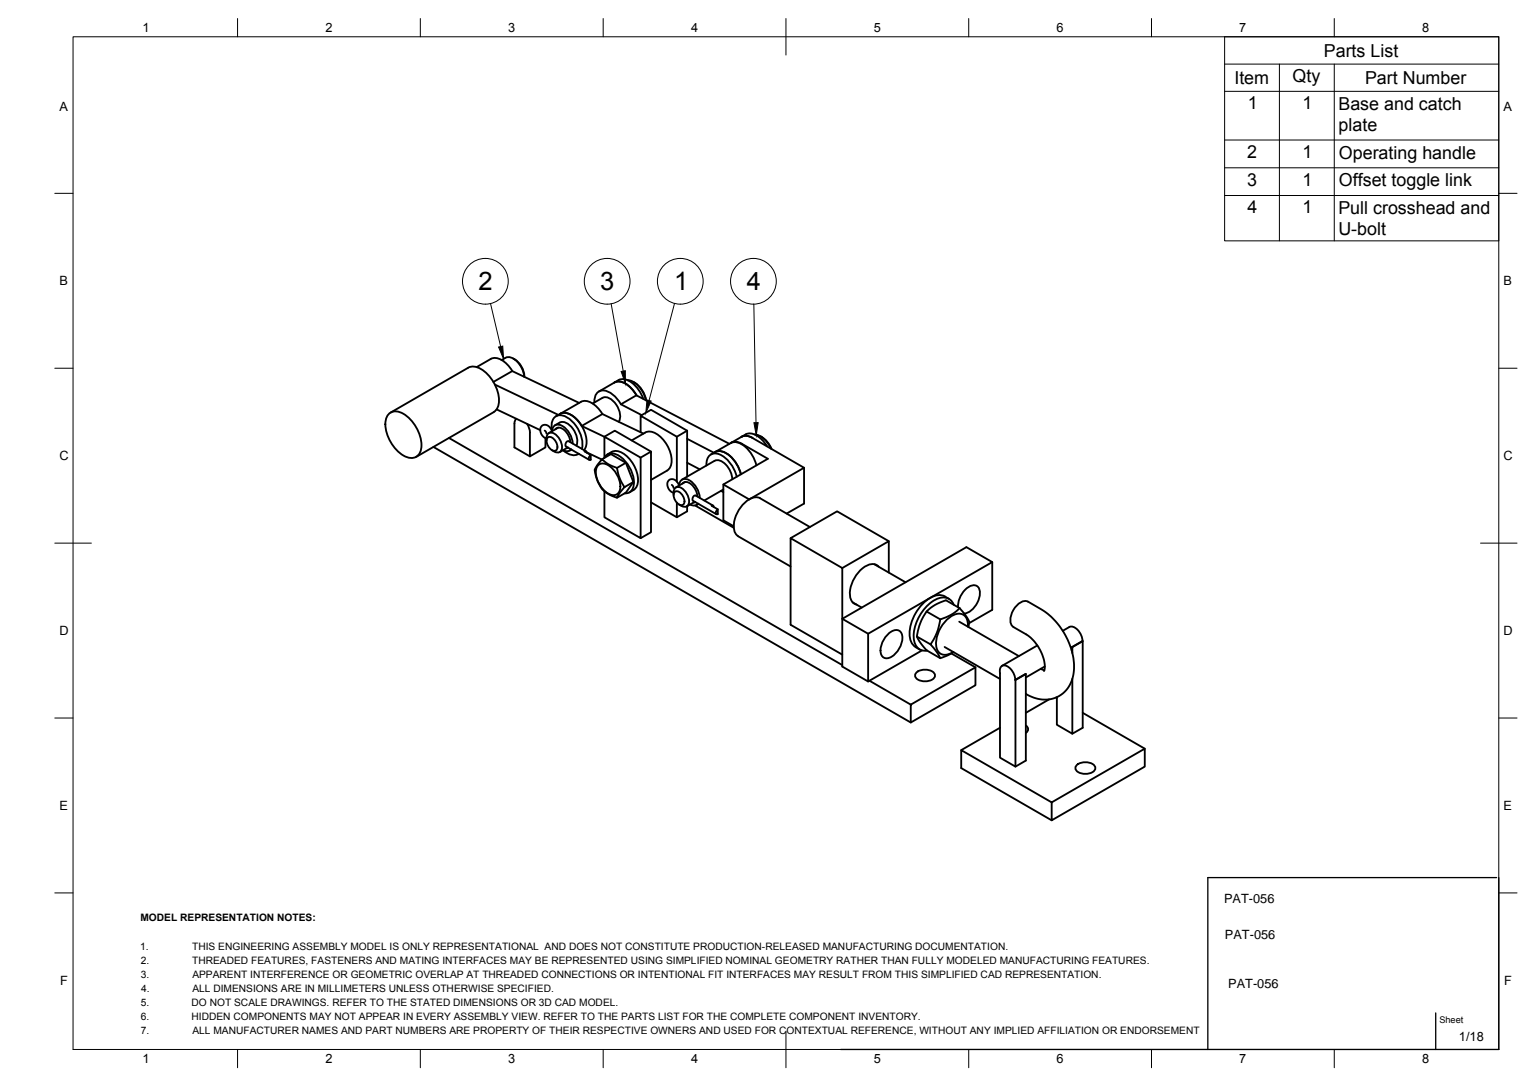
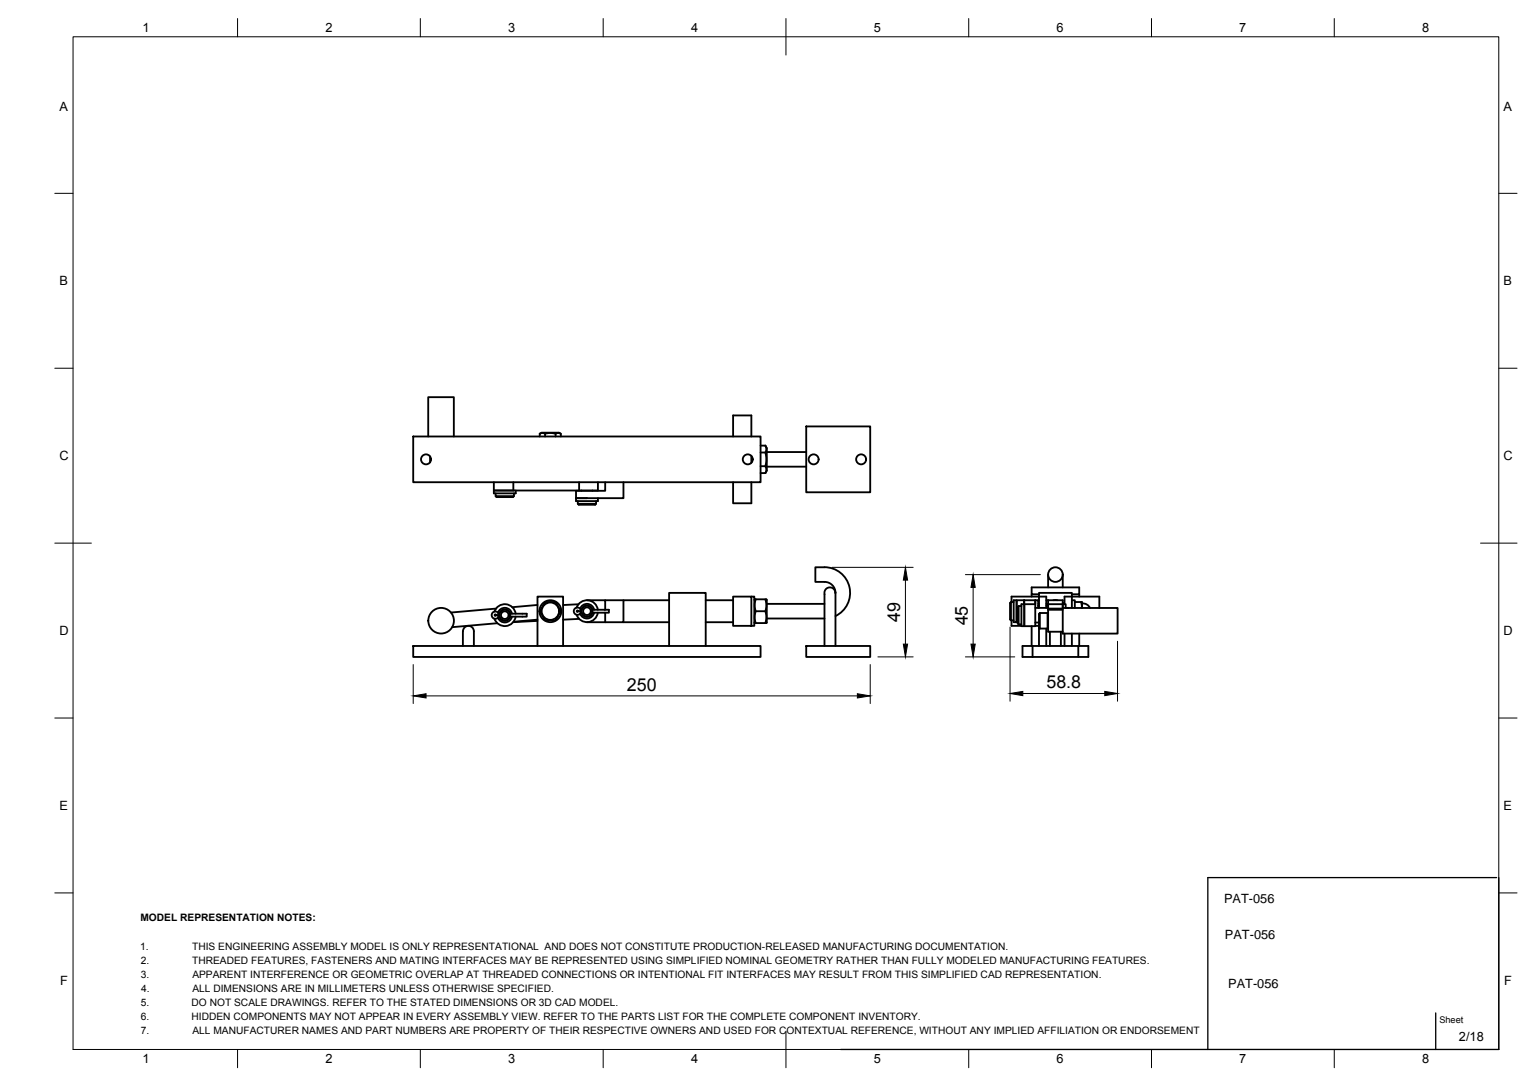
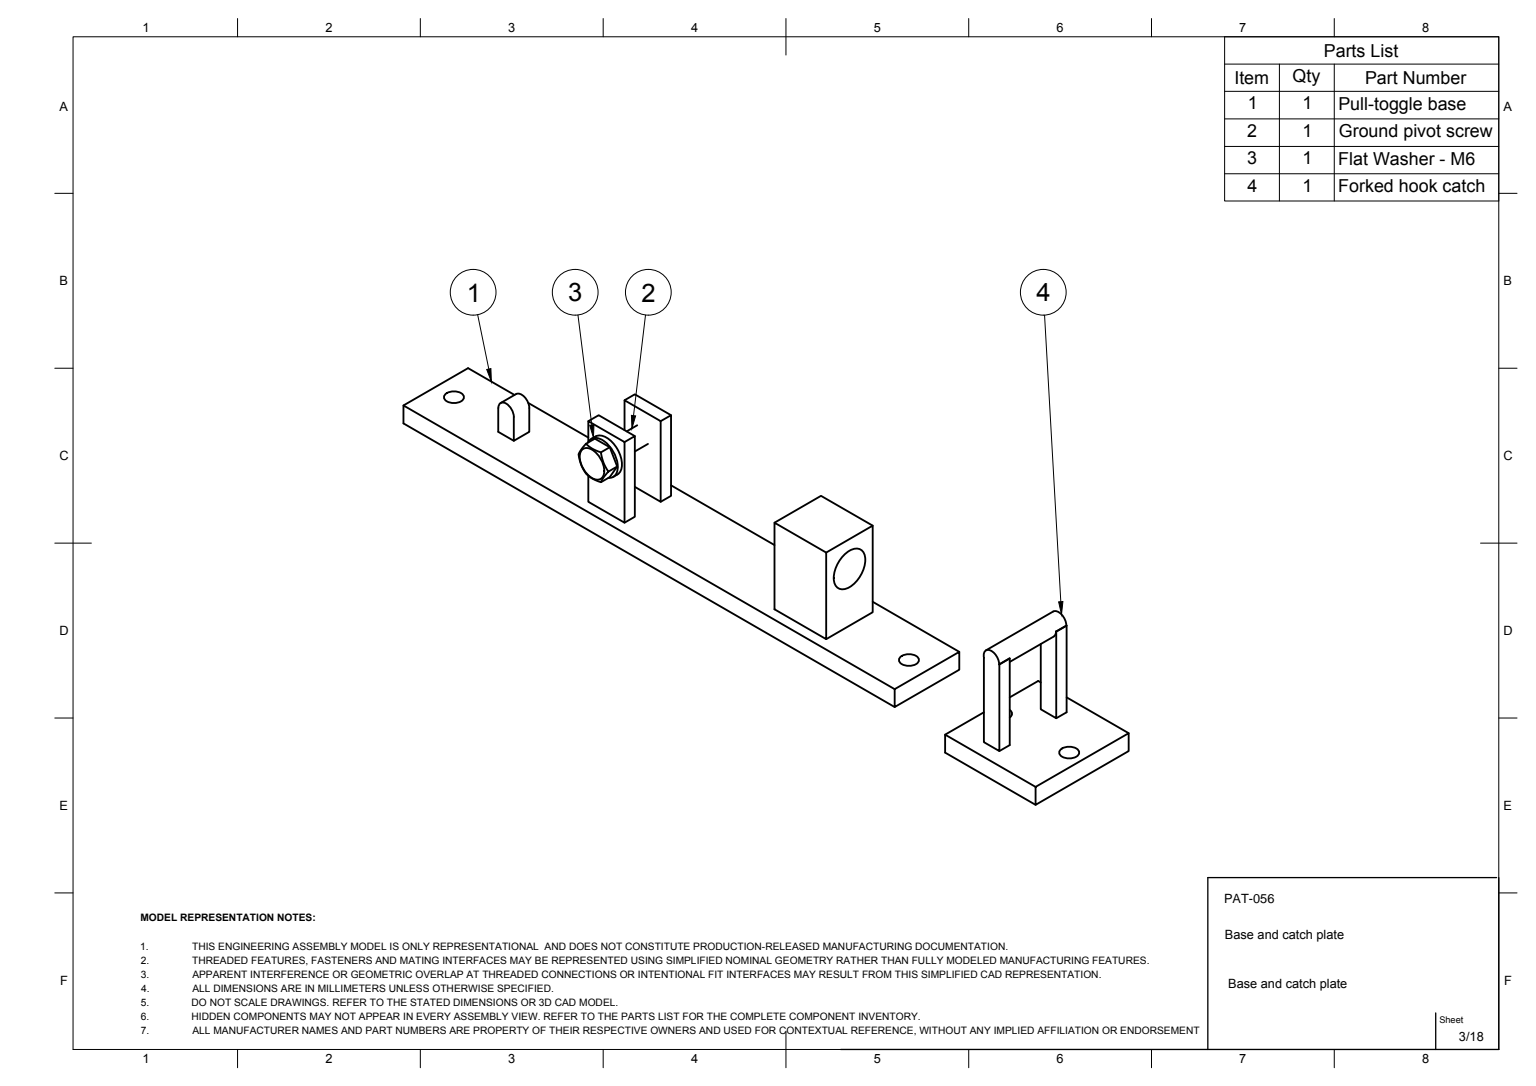
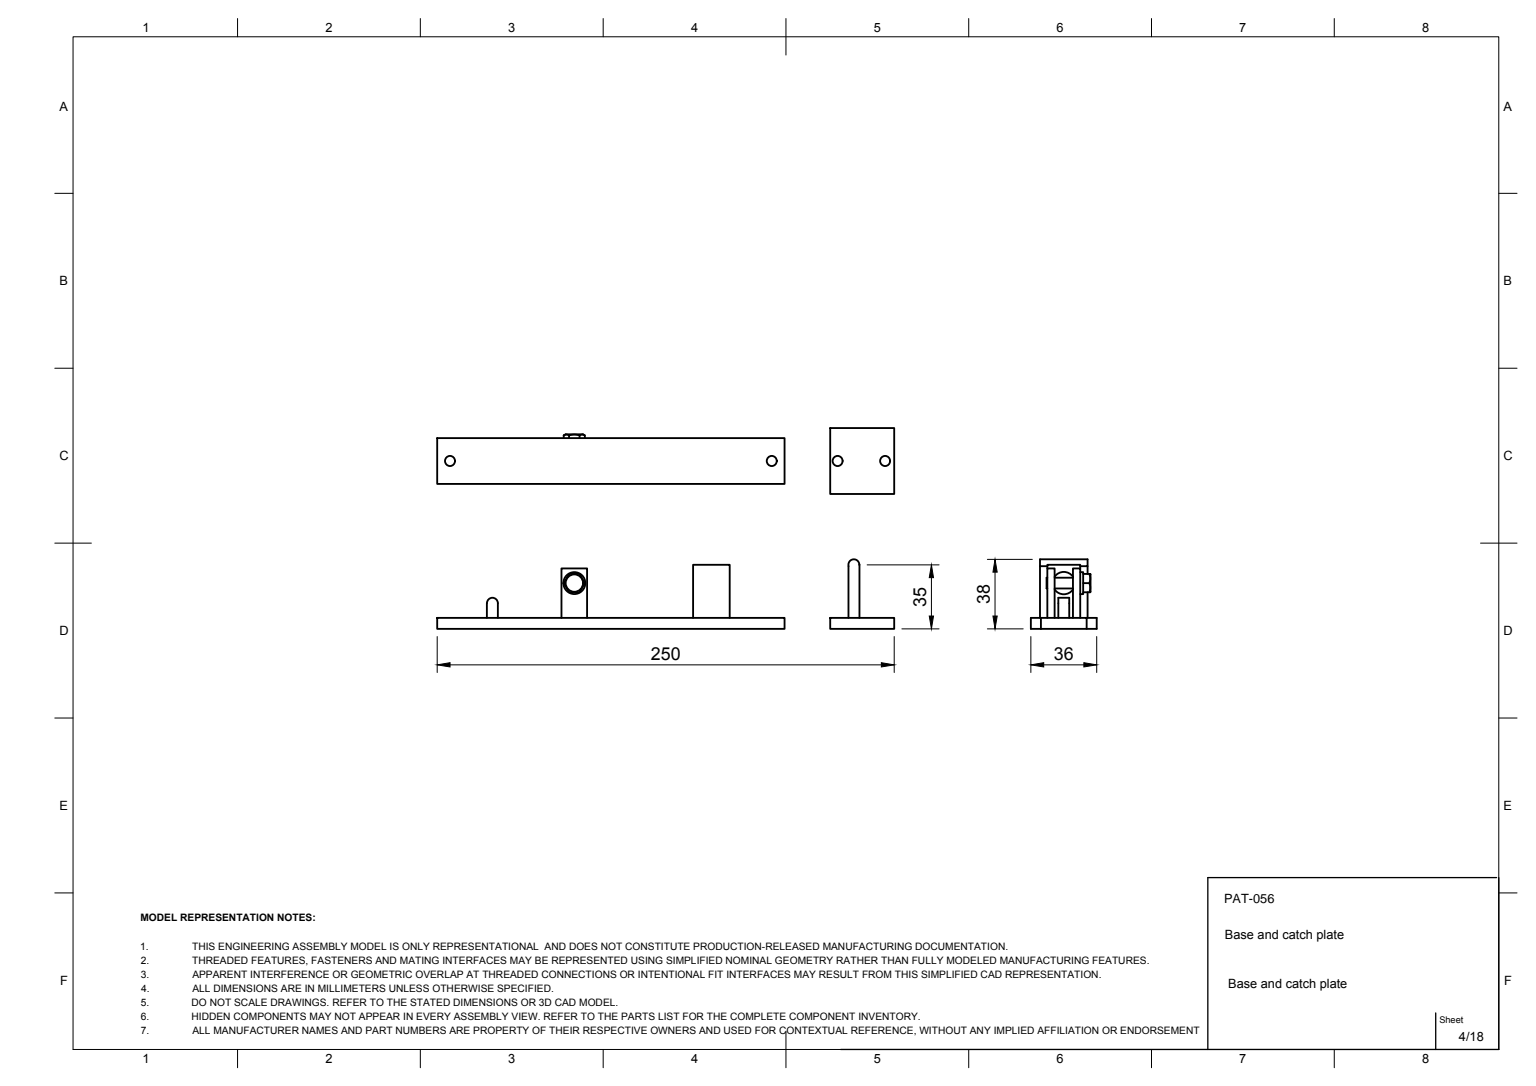
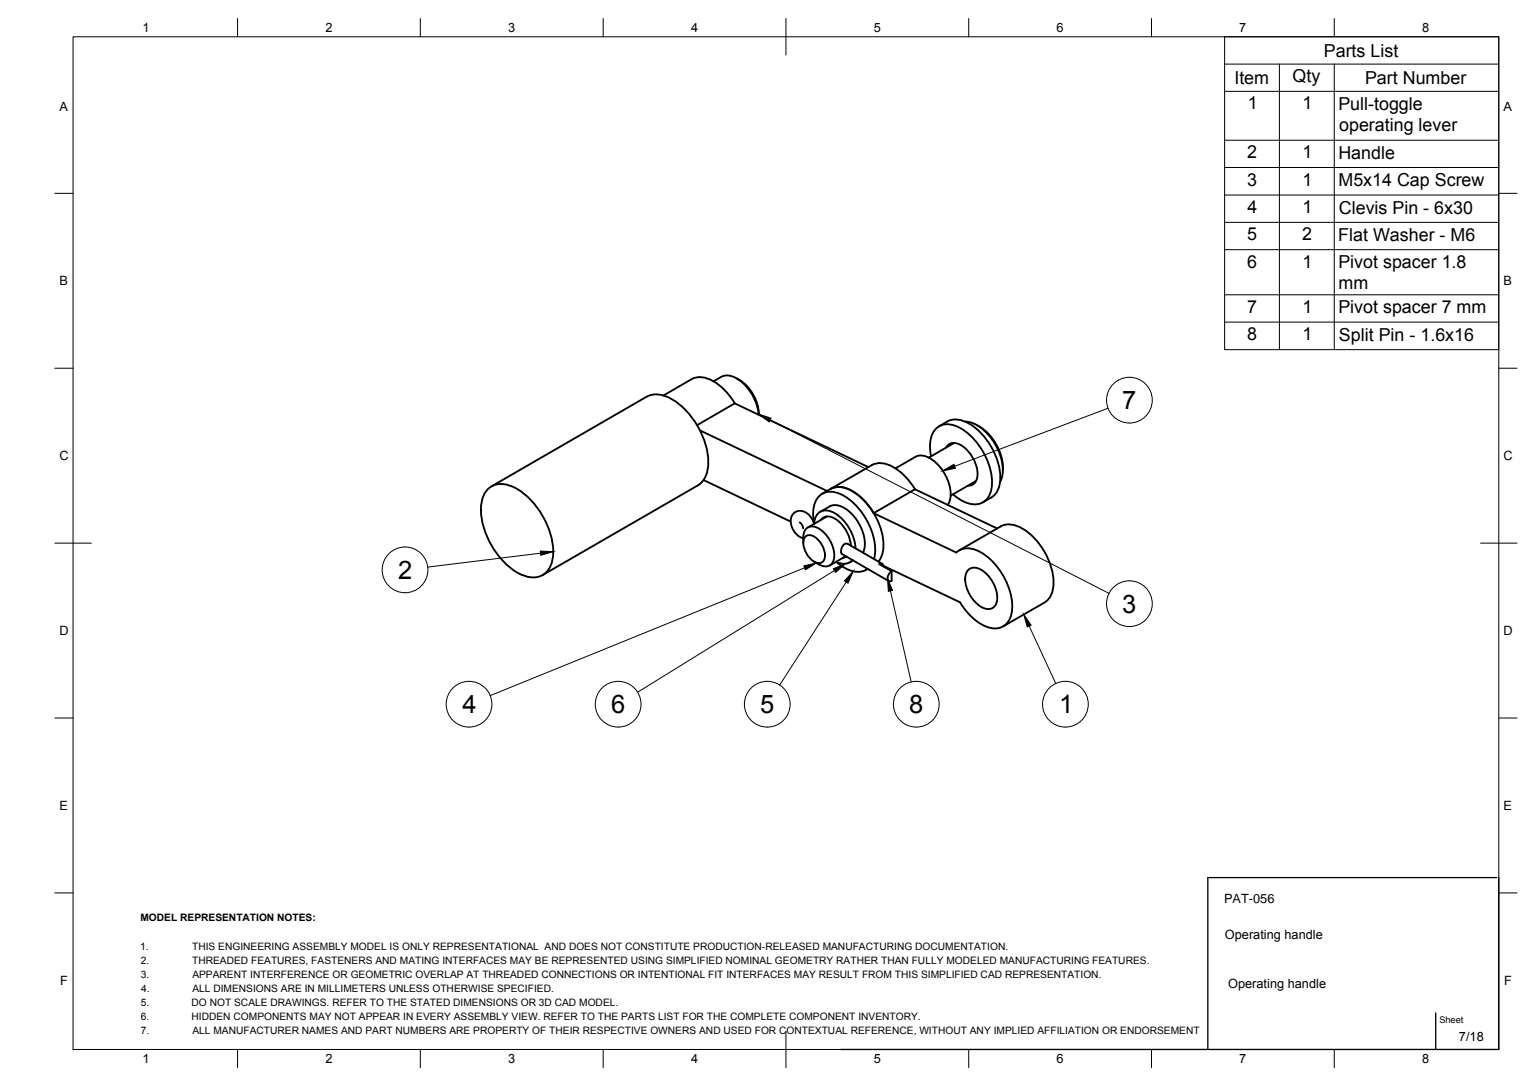
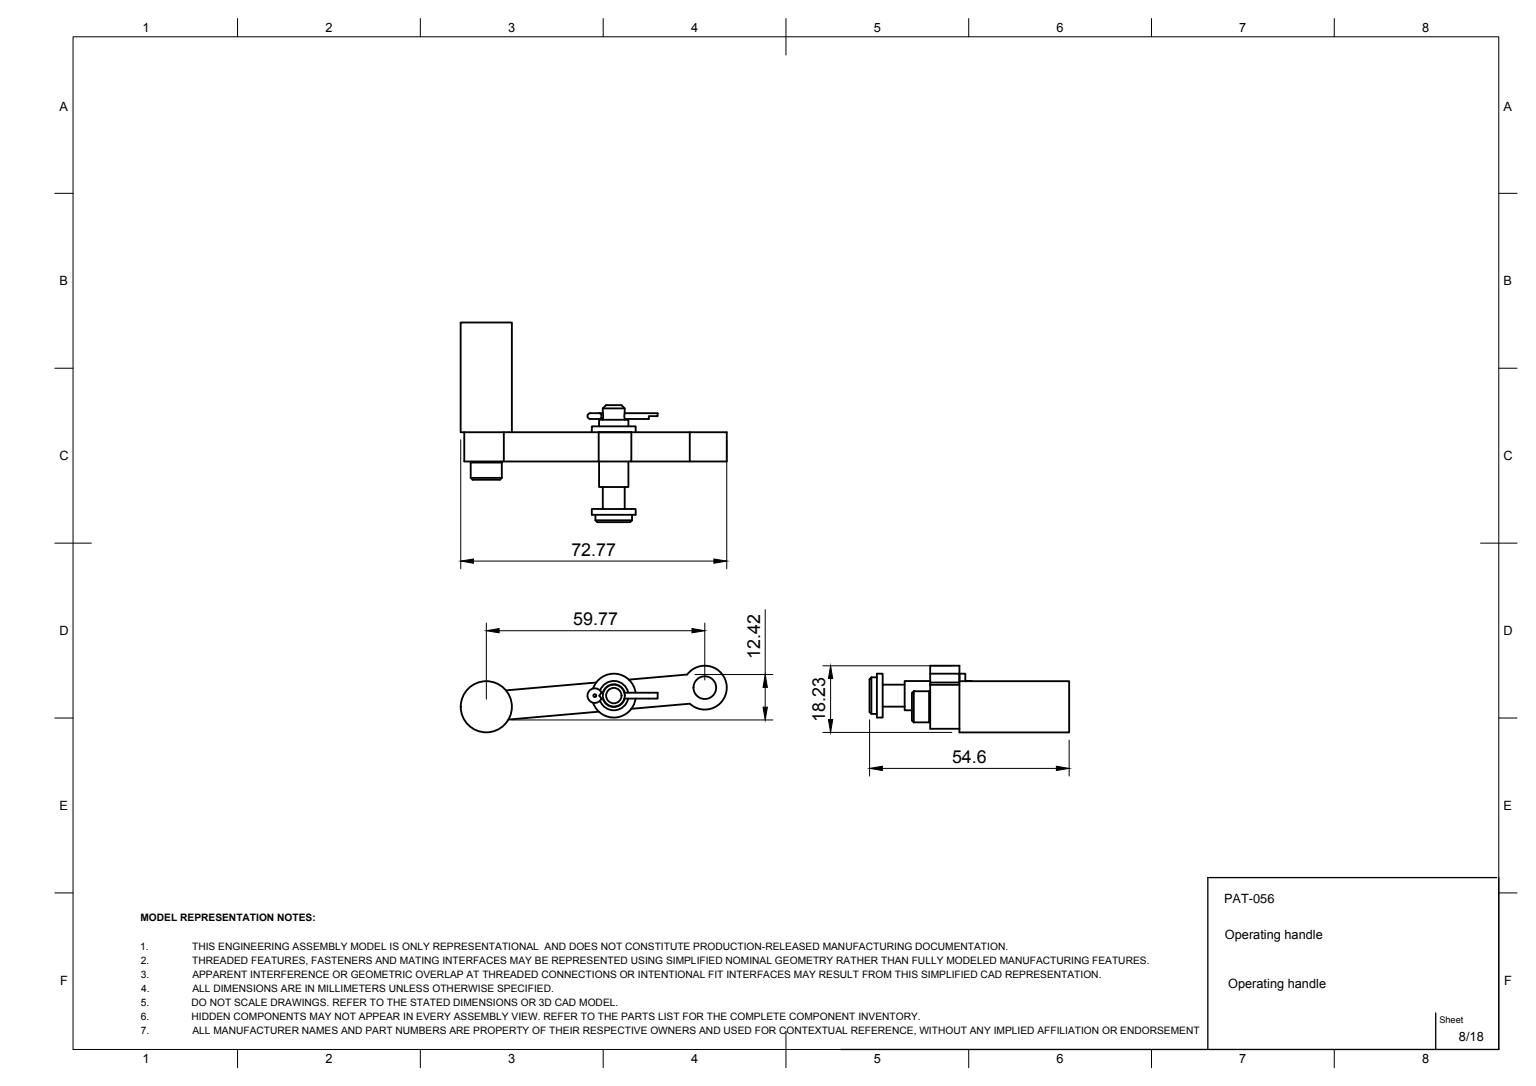
ISO-10303-21;
HEADER;
/* Generated by software containing ST-Developer
 * from STEP Tools, Inc. (www.steptools.com) 
 */

FILE_DESCRIPTION(
/* description */ ('Hook toggle clamp'),
/* implementation_level */ '2;1');

FILE_NAME(
/* name */ 'PAT-056',
/* time_stamp */ '2026-10-27T21:56:56-07:00',
/* author */ (''),
/* organization */ (''),
/* preprocessor_version */ 'ST-DEVELOPER v20.2',
/* originating_system */ 'Autodesk Translation Framework v15.17.0.0',
/* authorisation */ '');

FILE_SCHEMA (('AUTOMOTIVE_DESIGN { 1 0 10303 214 3 1 1 }'));
ENDSEC;

DATA;
#10=MECHANICAL_DESIGN_GEOMETRIC_PRESENTATION_REPRESENTATION('',(#189,#190,
#191,#192,#193,#194,#195,#196,#197,#198,#199,#200,#201,#202,#203,#204,#205),
#5458);
#11=TOROIDAL_SURFACE('',#3441,0.12,0.08);
#12=TOROIDAL_SURFACE('',#3465,1.,0.4);
#13=B_SPLINE_CURVE_WITH_KNOTS('',3,(#5084,#5085,#5086,#5087,#5088,#5089,
#5090,#5091,#5092,#5093),.UNSPECIFIED.,.F.,.F.,(4,2,2,2,4),(0.,0.0302963256060356,
0.0605926512120712,0.090883446720838,0.121174242229605),.UNSPECIFIED.);
#14=B_SPLINE_CURVE_WITH_KNOTS('',3,(#5096,#5097,#5098,#5099,#5100,#5101,
#5102,#5103,#5104,#5105,#5106,#5107,#5108,#5109,#5110,#5111,#5112,#5113,
#5114,#5115,#5116,#5117,#5118,#5119,#5120,#5121,#5122,#5123,#5124,#5125,
#5126,#5127,#5128,#5129),.UNSPECIFIED.,.T.,.F.,(4,2,2,2,2,2,2,2,2,2,2,2,
2,2,2,2,4),(0.,0.0302963256060358,0.0605926512120716,0.0908834467208383,
0.121174242229605,0.151465037738372,0.181755833247138,0.212052158853174,
0.24234848445921,0.272644810065246,0.302941135671282,0.333231931180048,
0.363522726688815,0.393813522197582,0.424104317706349,0.454400643312384,
0.48469696891842),.UNSPECIFIED.);
#15=B_SPLINE_CURVE_WITH_KNOTS('',3,(#5131,#5132,#5133,#5134,#5135,#5136,
#5137,#5138,#5139,#5140),.UNSPECIFIED.,.F.,.F.,(4,2,2,2,4),(0.363522726688815,
0.393813522197581,0.424104317706348,0.454400643312384,0.48469696891842),
 .UNSPECIFIED.);
#16=B_SPLINE_CURVE_WITH_KNOTS('',3,(#5141,#5142,#5143,#5144,#5145,#5146,
#5147,#5148,#5149,#5150,#5151,#5152,#5153,#5154,#5155,#5156,#5157,#5158),
 .UNSPECIFIED.,.F.,.F.,(4,2,2,2,2,2,2,2,4),(0.121174242229605,0.151465037738371,
0.181755833247138,0.212052158853174,0.24234848445921,0.272644810065246,
0.302941135671281,0.333231931180048,0.363522726688815),.UNSPECIFIED.);
#17=B_SPLINE_CURVE_WITH_KNOTS('',3,(#5209,#5210,#5211,#5212,#5213,#5214,
#5215,#5216,#5217,#5218,#5219,#5220,#5221,#5222,#5223,#5224,#5225,#5226,
#5227,#5228,#5229,#5230,#5231,#5232,#5233,#5234),.UNSPECIFIED.,.F.,.F.,
(4,2,2,2,2,2,2,2,2,2,2,2,4),(-0.00054581412719389,0.,0.0281583564005144,
0.0618496465371181,0.0905865724114538,0.120694112793616,0.144966158459363,
0.16923820412511,0.199345744507272,0.228082670381608,0.261773960518212,
0.289932316918681,0.290478131045882),.UNSPECIFIED.);
#18=B_SPLINE_CURVE_WITH_KNOTS('',3,(#5235,#5236,#5237,#5238,#5239,#5240,
#5241,#5242,#5243,#5244,#5245,#5246,#5247,#5248,#5249,#5250,#5251,#5252,
#5253,#5254,#5255,#5256,#5257,#5258,#5259,#5260),.UNSPECIFIED.,.F.,.F.,
(4,2,2,2,2,2,2,2,2,2,2,2,4),(-0.000545814127196571,0.,0.0281583564006391,
0.0618496465374156,0.0905865724118984,0.120694112794215,0.144966158460086,
0.169238204125958,0.199345744508275,0.228082670382758,0.261773960519534,
0.289932316920171,0.29047813104737),.UNSPECIFIED.);
#19=ITEM_DEFINED_TRANSFORMATION($,$,#3349,#3366);
#20=ITEM_DEFINED_TRANSFORMATION($,$,#3178,#3436);
#21=ITEM_DEFINED_TRANSFORMATION($,$,#3222,#3437);
#22=ITEM_DEFINED_TRANSFORMATION($,$,#3427,#3438);
#23=ITEM_DEFINED_TRANSFORMATION($,$,#3237,#3439);
#24=ITEM_DEFINED_TRANSFORMATION($,$,#3268,#3451);
#25=ITEM_DEFINED_TRANSFORMATION($,$,#3296,#3452);
#26=ITEM_DEFINED_TRANSFORMATION($,$,#3305,#3453);
#27=ITEM_DEFINED_TRANSFORMATION($,$,#3314,#3454);
#28=ITEM_DEFINED_TRANSFORMATION($,$,#3324,#3455);
#29=ITEM_DEFINED_TRANSFORMATION($,$,#3412,#3456);
#30=ITEM_DEFINED_TRANSFORMATION($,$,#3427,#3457);
#31=ITEM_DEFINED_TRANSFORMATION($,$,#3427,#3458);
#32=ITEM_DEFINED_TRANSFORMATION($,$,#3440,#3459);
#33=ITEM_DEFINED_TRANSFORMATION($,$,#3368,#3498);
#34=ITEM_DEFINED_TRANSFORMATION($,$,#3403,#3499);
#35=ITEM_DEFINED_TRANSFORMATION($,$,#3412,#3500);
#36=ITEM_DEFINED_TRANSFORMATION($,$,#3427,#3501);
#37=ITEM_DEFINED_TRANSFORMATION($,$,#3427,#3502);
#38=ITEM_DEFINED_TRANSFORMATION($,$,#3440,#3503);
#39=ITEM_DEFINED_TRANSFORMATION($,$,#3460,#3504);
#40=ITEM_DEFINED_TRANSFORMATION($,$,#3473,#3505);
#41=ITEM_DEFINED_TRANSFORMATION($,$,#3482,#3506);
#42=ITEM_DEFINED_TRANSFORMATION($,$,#3177,#3507);
#43=ITEM_DEFINED_TRANSFORMATION($,$,#3267,#3508);
#44=ITEM_DEFINED_TRANSFORMATION($,$,#3348,#3509);
#45=ITEM_DEFINED_TRANSFORMATION($,$,#3367,#3510);
#46=(
REPRESENTATION_RELATIONSHIP($,$,#5546,#5545)
REPRESENTATION_RELATIONSHIP_WITH_TRANSFORMATION(#19)
SHAPE_REPRESENTATION_RELATIONSHIP()
);
#47=(
REPRESENTATION_RELATIONSHIP($,$,#5536,#5535)
REPRESENTATION_RELATIONSHIP_WITH_TRANSFORMATION(#20)
SHAPE_REPRESENTATION_RELATIONSHIP()
);
#48=(
REPRESENTATION_RELATIONSHIP($,$,#5537,#5535)
REPRESENTATION_RELATIONSHIP_WITH_TRANSFORMATION(#21)
SHAPE_REPRESENTATION_RELATIONSHIP()
);
#49=(
REPRESENTATION_RELATIONSHIP($,$,#5551,#5535)
REPRESENTATION_RELATIONSHIP_WITH_TRANSFORMATION(#22)
SHAPE_REPRESENTATION_RELATIONSHIP()
);
#50=(
REPRESENTATION_RELATIONSHIP($,$,#5538,#5535)
REPRESENTATION_RELATIONSHIP_WITH_TRANSFORMATION(#23)
SHAPE_REPRESENTATION_RELATIONSHIP()
);
#51=(
REPRESENTATION_RELATIONSHIP($,$,#5540,#5539)
REPRESENTATION_RELATIONSHIP_WITH_TRANSFORMATION(#24)
SHAPE_REPRESENTATION_RELATIONSHIP()
);
#52=(
REPRESENTATION_RELATIONSHIP($,$,#5541,#5539)
REPRESENTATION_RELATIONSHIP_WITH_TRANSFORMATION(#25)
SHAPE_REPRESENTATION_RELATIONSHIP()
);
#53=(
REPRESENTATION_RELATIONSHIP($,$,#5542,#5539)
REPRESENTATION_RELATIONSHIP_WITH_TRANSFORMATION(#26)
SHAPE_REPRESENTATION_RELATIONSHIP()
);
#54=(
REPRESENTATION_RELATIONSHIP($,$,#5543,#5539)
REPRESENTATION_RELATIONSHIP_WITH_TRANSFORMATION(#27)
SHAPE_REPRESENTATION_RELATIONSHIP()
);
#55=(
REPRESENTATION_RELATIONSHIP($,$,#5544,#5539)
REPRESENTATION_RELATIONSHIP_WITH_TRANSFORMATION(#28)
SHAPE_REPRESENTATION_RELATIONSHIP()
);
#56=(
REPRESENTATION_RELATIONSHIP($,$,#5550,#5539)
REPRESENTATION_RELATIONSHIP_WITH_TRANSFORMATION(#29)
SHAPE_REPRESENTATION_RELATIONSHIP()
);
#57=(
REPRESENTATION_RELATIONSHIP($,$,#5551,#5539)
REPRESENTATION_RELATIONSHIP_WITH_TRANSFORMATION(#30)
SHAPE_REPRESENTATION_RELATIONSHIP()
);
#58=(
REPRESENTATION_RELATIONSHIP($,$,#5551,#5539)
REPRESENTATION_RELATIONSHIP_WITH_TRANSFORMATION(#31)
SHAPE_REPRESENTATION_RELATIONSHIP()
);
#59=(
REPRESENTATION_RELATIONSHIP($,$,#5552,#5539)
REPRESENTATION_RELATIONSHIP_WITH_TRANSFORMATION(#32)
SHAPE_REPRESENTATION_RELATIONSHIP()
);
#60=(
REPRESENTATION_RELATIONSHIP($,$,#5548,#5547)
REPRESENTATION_RELATIONSHIP_WITH_TRANSFORMATION(#33)
SHAPE_REPRESENTATION_RELATIONSHIP()
);
#61=(
REPRESENTATION_RELATIONSHIP($,$,#5549,#5547)
REPRESENTATION_RELATIONSHIP_WITH_TRANSFORMATION(#34)
SHAPE_REPRESENTATION_RELATIONSHIP()
);
#62=(
REPRESENTATION_RELATIONSHIP($,$,#5550,#5547)
REPRESENTATION_RELATIONSHIP_WITH_TRANSFORMATION(#35)
SHAPE_REPRESENTATION_RELATIONSHIP()
);
#63=(
REPRESENTATION_RELATIONSHIP($,$,#5551,#5547)
REPRESENTATION_RELATIONSHIP_WITH_TRANSFORMATION(#36)
SHAPE_REPRESENTATION_RELATIONSHIP()
);
#64=(
REPRESENTATION_RELATIONSHIP($,$,#5551,#5547)
REPRESENTATION_RELATIONSHIP_WITH_TRANSFORMATION(#37)
SHAPE_REPRESENTATION_RELATIONSHIP()
);
#65=(
REPRESENTATION_RELATIONSHIP($,$,#5552,#5547)
REPRESENTATION_RELATIONSHIP_WITH_TRANSFORMATION(#38)
SHAPE_REPRESENTATION_RELATIONSHIP()
);
#66=(
REPRESENTATION_RELATIONSHIP($,$,#5553,#5547)
REPRESENTATION_RELATIONSHIP_WITH_TRANSFORMATION(#39)
SHAPE_REPRESENTATION_RELATIONSHIP()
);
#67=(
REPRESENTATION_RELATIONSHIP($,$,#5554,#5547)
REPRESENTATION_RELATIONSHIP_WITH_TRANSFORMATION(#40)
SHAPE_REPRESENTATION_RELATIONSHIP()
);
#68=(
REPRESENTATION_RELATIONSHIP($,$,#5555,#5547)
REPRESENTATION_RELATIONSHIP_WITH_TRANSFORMATION(#41)
SHAPE_REPRESENTATION_RELATIONSHIP()
);
#69=(
REPRESENTATION_RELATIONSHIP($,$,#5535,#5534)
REPRESENTATION_RELATIONSHIP_WITH_TRANSFORMATION(#42)
SHAPE_REPRESENTATION_RELATIONSHIP()
);
#70=(
REPRESENTATION_RELATIONSHIP($,$,#5539,#5534)
REPRESENTATION_RELATIONSHIP_WITH_TRANSFORMATION(#43)
SHAPE_REPRESENTATION_RELATIONSHIP()
);
#71=(
REPRESENTATION_RELATIONSHIP($,$,#5545,#5534)
REPRESENTATION_RELATIONSHIP_WITH_TRANSFORMATION(#44)
SHAPE_REPRESENTATION_RELATIONSHIP()
);
#72=(
REPRESENTATION_RELATIONSHIP($,$,#5547,#5534)
REPRESENTATION_RELATIONSHIP_WITH_TRANSFORMATION(#45)
SHAPE_REPRESENTATION_RELATIONSHIP()
);
#73=CONTEXT_DEPENDENT_SHAPE_REPRESENTATION(#46,#5498);
#74=CONTEXT_DEPENDENT_SHAPE_REPRESENTATION(#47,#5504);
#75=CONTEXT_DEPENDENT_SHAPE_REPRESENTATION(#48,#5505);
#76=CONTEXT_DEPENDENT_SHAPE_REPRESENTATION(#49,#5506);
#77=CONTEXT_DEPENDENT_SHAPE_REPRESENTATION(#50,#5507);
#78=CONTEXT_DEPENDENT_SHAPE_REPRESENTATION(#51,#5509);
#79=CONTEXT_DEPENDENT_SHAPE_REPRESENTATION(#52,#5510);
#80=CONTEXT_DEPENDENT_SHAPE_REPRESENTATION(#53,#5511);
#81=CONTEXT_DEPENDENT_SHAPE_REPRESENTATION(#54,#5512);
#82=CONTEXT_DEPENDENT_SHAPE_REPRESENTATION(#55,#5513);
#83=CONTEXT_DEPENDENT_SHAPE_REPRESENTATION(#56,#5514);
#84=CONTEXT_DEPENDENT_SHAPE_REPRESENTATION(#57,#5515);
#85=CONTEXT_DEPENDENT_SHAPE_REPRESENTATION(#58,#5516);
#86=CONTEXT_DEPENDENT_SHAPE_REPRESENTATION(#59,#5517);
#87=CONTEXT_DEPENDENT_SHAPE_REPRESENTATION(#60,#5521);
#88=CONTEXT_DEPENDENT_SHAPE_REPRESENTATION(#61,#5522);
#89=CONTEXT_DEPENDENT_SHAPE_REPRESENTATION(#62,#5523);
#90=CONTEXT_DEPENDENT_SHAPE_REPRESENTATION(#63,#5524);
#91=CONTEXT_DEPENDENT_SHAPE_REPRESENTATION(#64,#5525);
#92=CONTEXT_DEPENDENT_SHAPE_REPRESENTATION(#65,#5526);
#93=CONTEXT_DEPENDENT_SHAPE_REPRESENTATION(#66,#5527);
#94=CONTEXT_DEPENDENT_SHAPE_REPRESENTATION(#67,#5528);
#95=CONTEXT_DEPENDENT_SHAPE_REPRESENTATION(#68,#5529);
#96=CONTEXT_DEPENDENT_SHAPE_REPRESENTATION(#69,#5530);
#97=CONTEXT_DEPENDENT_SHAPE_REPRESENTATION(#70,#5531);
#98=CONTEXT_DEPENDENT_SHAPE_REPRESENTATION(#71,#5532);
#99=CONTEXT_DEPENDENT_SHAPE_REPRESENTATION(#72,#5533);
#100=NEXT_ASSEMBLY_USAGE_OCCURRENCE('Offset pull link:1',
'Offset pull link:1','Offset pull link:1',#5568,#5569,
'Offset pull link:1');
#101=NEXT_ASSEMBLY_USAGE_OCCURRENCE('Pull-toggle base:1',
'Pull-toggle base:1','Pull-toggle base:1',#5558,#5559,
'Pull-toggle base:1');
#102=NEXT_ASSEMBLY_USAGE_OCCURRENCE('Ground pivot screw:2',
'Ground pivot screw:2','Ground pivot screw:2',#5558,#5560,
'Ground pivot screw:2');
#103=NEXT_ASSEMBLY_USAGE_OCCURRENCE('Flat Washer - M6:2',
'Flat Washer - M6:2','Flat Washer - M6:2',#5558,#5574,
'Flat Washer - M6:2');
#104=NEXT_ASSEMBLY_USAGE_OCCURRENCE('Forked hook catch:1',
'Forked hook catch:1','Forked hook catch:1',#5558,#5561,
'Forked hook catch:1');
#105=NEXT_ASSEMBLY_USAGE_OCCURRENCE('Pull-toggle operating lever:1',
'Pull-toggle operating lever:1','Pull-toggle operating lever:1',#5562,#5563,
'Pull-toggle operating lever:1');
#106=NEXT_ASSEMBLY_USAGE_OCCURRENCE('Pivot spacer 1.8 mm:1',
'Pivot spacer 1.8 mm:1','Pivot spacer 1.8 mm:1',#5562,#5564,
'Pivot spacer 1.8 mm:1');
#107=NEXT_ASSEMBLY_USAGE_OCCURRENCE('Pivot spacer 7 mm:1',
'Pivot spacer 7 mm:1','Pivot spacer 7 mm:1',#5562,#5565,
'Pivot spacer 7 mm:1');
#108=NEXT_ASSEMBLY_USAGE_OCCURRENCE('Handle:2','Handle:2','Handle:2',#5562,
#5566,'Handle:2');
#109=NEXT_ASSEMBLY_USAGE_OCCURRENCE('M5x14 Cap Screw:2',
'M5x14 Cap Screw:2','M5x14 Cap Screw:2',#5562,#5567,'M5x14 Cap Screw:2');
#110=NEXT_ASSEMBLY_USAGE_OCCURRENCE('Clevis Pin - 6x30:2',
'Clevis Pin - 6x30:2','Clevis Pin - 6x30:2',#5562,#5573,
'Clevis Pin - 6x30:2');
#111=NEXT_ASSEMBLY_USAGE_OCCURRENCE('Flat Washer - M6:3',
'Flat Washer - M6:3','Flat Washer - M6:3',#5562,#5574,
'Flat Washer - M6:3');
#112=NEXT_ASSEMBLY_USAGE_OCCURRENCE('Flat Washer - M6:4',
'Flat Washer - M6:4','Flat Washer - M6:4',#5562,#5574,
'Flat Washer - M6:4');
#113=NEXT_ASSEMBLY_USAGE_OCCURRENCE('Split Pin - 1.6x16:2',
'Split Pin - 1.6x16:2','Split Pin - 1.6x16:2',#5562,#5575,
'Split Pin - 1.6x16:2');
#114=NEXT_ASSEMBLY_USAGE_OCCURRENCE('Threaded hook crosshead:1',
'Threaded hook crosshead:1','Threaded hook crosshead:1',#5570,#5571,
'Threaded hook crosshead:1');
#115=NEXT_ASSEMBLY_USAGE_OCCURRENCE('Pivot spacer 12.6 mm:1',
'Pivot spacer 12.6 mm:1','Pivot spacer 12.6 mm:1',#5570,#5572,
'Pivot spacer 12.6 mm:1');
#116=NEXT_ASSEMBLY_USAGE_OCCURRENCE('Clevis Pin - 6x30:3',
'Clevis Pin - 6x30:3','Clevis Pin - 6x30:3',#5570,#5573,
'Clevis Pin - 6x30:3');
#117=NEXT_ASSEMBLY_USAGE_OCCURRENCE('Flat Washer - M6:5',
'Flat Washer - M6:5','Flat Washer - M6:5',#5570,#5574,
'Flat Washer - M6:5');
#118=NEXT_ASSEMBLY_USAGE_OCCURRENCE('Flat Washer - M6:6',
'Flat Washer - M6:6','Flat Washer - M6:6',#5570,#5574,
'Flat Washer - M6:6');
#119=NEXT_ASSEMBLY_USAGE_OCCURRENCE('Split Pin - 1.6x16:3',
'Split Pin - 1.6x16:3','Split Pin - 1.6x16:3',#5570,#5575,
'Split Pin - 1.6x16:3');
#120=NEXT_ASSEMBLY_USAGE_OCCURRENCE(
'Adjustable eight millimetre hook:1',
'Adjustable eight millimetre hook:1',
'Adjustable eight millimetre hook:1',#5570,#5576,
'Adjustable eight millimetre hook:1');
#121=NEXT_ASSEMBLY_USAGE_OCCURRENCE('Flat Washer - M8:2',
'Flat Washer - M8:2','Flat Washer - M8:2',#5570,#5577,
'Flat Washer - M8:2');
#122=NEXT_ASSEMBLY_USAGE_OCCURRENCE('Hex Nut - M8:2','Hex Nut - M8:2',
'Hex Nut - M8:2',#5570,#5578,'Hex Nut - M8:2');
#123=NEXT_ASSEMBLY_USAGE_OCCURRENCE('Base and catch plate:1',
'Base and catch plate:1','Base and catch plate:1',#5557,#5558,
'Base and catch plate:1');
#124=NEXT_ASSEMBLY_USAGE_OCCURRENCE('Operating handle:1',
'Operating handle:1','Operating handle:1',#5557,#5562,
'Operating handle:1');
#125=NEXT_ASSEMBLY_USAGE_OCCURRENCE('Offset toggle link:1',
'Offset toggle link:1','Offset toggle link:1',#5557,#5568,
'Offset toggle link:1');
#126=NEXT_ASSEMBLY_USAGE_OCCURRENCE('Pull crosshead and U-bolt:1',
'Pull crosshead and U-bolt:1','Pull crosshead and U-bolt:1',#5557,#5570,
'Pull crosshead and U-bolt:1');
#127=ORIENTED_CLOSED_SHELL('',*,#2977,.F.);
#128=BREP_WITH_VOIDS('Body1',#2978,(#127));
#129=(
BOUNDED_CURVE()
B_SPLINE_CURVE(2,(#4591,#4592,#4593),.UNSPECIFIED.,.F.,.F.)
B_SPLINE_CURVE_WITH_KNOTS((3,3),(0.144988513094728,0.791574906712449),
 .UNSPECIFIED.)
CURVE()
GEOMETRIC_REPRESENTATION_ITEM()
RATIONAL_B_SPLINE_CURVE((1.09282032302755,1.26188021535082,1.09282032302931))
REPRESENTATION_ITEM('')
);
#130=(
BOUNDED_CURVE()
B_SPLINE_CURVE(2,(#4595,#4596,#4597),.UNSPECIFIED.,.F.,.F.)
B_SPLINE_CURVE_WITH_KNOTS((3,3),(0.144988513094728,0.791574906712449),
 .UNSPECIFIED.)
CURVE()
GEOMETRIC_REPRESENTATION_ITEM()
RATIONAL_B_SPLINE_CURVE((1.09282032302755,1.26188021535082,1.09282032302931))
REPRESENTATION_ITEM('')
);
#131=(
BOUNDED_CURVE()
B_SPLINE_CURVE(2,(#4599,#4600,#4601),.UNSPECIFIED.,.F.,.F.)
B_SPLINE_CURVE_WITH_KNOTS((3,3),(0.144988513094728,0.791574906712449),
 .UNSPECIFIED.)
CURVE()
GEOMETRIC_REPRESENTATION_ITEM()
RATIONAL_B_SPLINE_CURVE((1.09282032302755,1.26188021535082,1.09282032302931))
REPRESENTATION_ITEM('')
);
#132=(
BOUNDED_CURVE()
B_SPLINE_CURVE(2,(#4603,#4604,#4605),.UNSPECIFIED.,.F.,.F.)
B_SPLINE_CURVE_WITH_KNOTS((3,3),(0.144988513094728,0.791574906712449),
 .UNSPECIFIED.)
CURVE()
GEOMETRIC_REPRESENTATION_ITEM()
RATIONAL_B_SPLINE_CURVE((1.09282032302755,1.26188021535082,1.09282032302931))
REPRESENTATION_ITEM('')
);
#133=(
BOUNDED_CURVE()
B_SPLINE_CURVE(2,(#4607,#4608,#4609),.UNSPECIFIED.,.F.,.F.)
B_SPLINE_CURVE_WITH_KNOTS((3,3),(0.144988513094728,0.791574906712449),
 .UNSPECIFIED.)
CURVE()
GEOMETRIC_REPRESENTATION_ITEM()
RATIONAL_B_SPLINE_CURVE((1.09282032302755,1.26188021535082,1.09282032302931))
REPRESENTATION_ITEM('')
);
#134=(
BOUNDED_CURVE()
B_SPLINE_CURVE(2,(#4610,#4611,#4612),.UNSPECIFIED.,.F.,.F.)
B_SPLINE_CURVE_WITH_KNOTS((3,3),(0.144988513094727,0.791574906712449),
 .UNSPECIFIED.)
CURVE()
GEOMETRIC_REPRESENTATION_ITEM()
RATIONAL_B_SPLINE_CURVE((1.09282032302755,1.26188021535082,1.09282032302931))
REPRESENTATION_ITEM('')
);
#135=(
BOUNDED_CURVE()
B_SPLINE_CURVE(2,(#5327,#5328,#5329),.UNSPECIFIED.,.F.,.F.)
B_SPLINE_CURVE_WITH_KNOTS((3,3),(0.14973948338295,0.97160236658079),
 .UNSPECIFIED.)
CURVE()
GEOMETRIC_REPRESENTATION_ITEM()
RATIONAL_B_SPLINE_CURVE((1.07140024848292,1.23714644374248,1.07140024848292))
REPRESENTATION_ITEM('')
);
#136=(
BOUNDED_CURVE()
B_SPLINE_CURVE(2,(#5331,#5332,#5333),.UNSPECIFIED.,.F.,.F.)
B_SPLINE_CURVE_WITH_KNOTS((3,3),(0.14973948338295,0.971602366580789),
 .UNSPECIFIED.)
CURVE()
GEOMETRIC_REPRESENTATION_ITEM()
RATIONAL_B_SPLINE_CURVE((1.07140024848292,1.23714644374248,1.07140024848292))
REPRESENTATION_ITEM('')
);
#137=(
BOUNDED_CURVE()
B_SPLINE_CURVE(2,(#5338,#5339,#5340),.UNSPECIFIED.,.F.,.F.)
B_SPLINE_CURVE_WITH_KNOTS((3,3),(0.14973948338295,0.97160236658079),
 .UNSPECIFIED.)
CURVE()
GEOMETRIC_REPRESENTATION_ITEM()
RATIONAL_B_SPLINE_CURVE((1.07140024848292,1.23714644374248,1.07140024848292))
REPRESENTATION_ITEM('')
);
#138=(
BOUNDED_CURVE()
B_SPLINE_CURVE(2,(#5342,#5343,#5344),.UNSPECIFIED.,.F.,.F.)
B_SPLINE_CURVE_WITH_KNOTS((3,3),(0.14973948338295,0.97160236658079),
 .UNSPECIFIED.)
CURVE()
GEOMETRIC_REPRESENTATION_ITEM()
RATIONAL_B_SPLINE_CURVE((1.07140024848292,1.23714644374248,1.07140024848292))
REPRESENTATION_ITEM('')
);
#139=(
BOUNDED_CURVE()
B_SPLINE_CURVE(2,(#5346,#5347,#5348),.UNSPECIFIED.,.F.,.F.)
B_SPLINE_CURVE_WITH_KNOTS((3,3),(0.14973948338295,0.971602366580789),
 .UNSPECIFIED.)
CURVE()
GEOMETRIC_REPRESENTATION_ITEM()
RATIONAL_B_SPLINE_CURVE((1.07140024848292,1.23714644374248,1.07140024848292))
REPRESENTATION_ITEM('')
);
#140=(
BOUNDED_CURVE()
B_SPLINE_CURVE(2,(#5349,#5350,#5351),.UNSPECIFIED.,.F.,.F.)
B_SPLINE_CURVE_WITH_KNOTS((3,3),(0.14973948338295,0.97160236658079),
 .UNSPECIFIED.)
CURVE()
GEOMETRIC_REPRESENTATION_ITEM()
RATIONAL_B_SPLINE_CURVE((1.07140024848292,1.23714644374248,1.07140024848292))
REPRESENTATION_ITEM('')
);
#141=(
BOUNDED_CURVE()
B_SPLINE_CURVE(2,(#5358,#5359,#5360),.UNSPECIFIED.,.F.,.F.)
B_SPLINE_CURVE_WITH_KNOTS((3,3),(0.14973948338295,0.97160236658079),
 .UNSPECIFIED.)
CURVE()
GEOMETRIC_REPRESENTATION_ITEM()
RATIONAL_B_SPLINE_CURVE((1.07140024848292,1.23714644374248,1.07140024848292))
REPRESENTATION_ITEM('')
);
#142=(
BOUNDED_CURVE()
B_SPLINE_CURVE(2,(#5362,#5363,#5364),.UNSPECIFIED.,.F.,.F.)
B_SPLINE_CURVE_WITH_KNOTS((3,3),(0.14973948338295,0.97160236658079),
 .UNSPECIFIED.)
CURVE()
GEOMETRIC_REPRESENTATION_ITEM()
RATIONAL_B_SPLINE_CURVE((1.07140024848292,1.23714644374248,1.07140024848292))
REPRESENTATION_ITEM('')
);
#143=(
BOUNDED_CURVE()
B_SPLINE_CURVE(2,(#5366,#5367,#5368),.UNSPECIFIED.,.F.,.F.)
B_SPLINE_CURVE_WITH_KNOTS((3,3),(0.14973948338295,0.971602366580789),
 .UNSPECIFIED.)
CURVE()
GEOMETRIC_REPRESENTATION_ITEM()
RATIONAL_B_SPLINE_CURVE((1.07140024848292,1.23714644374248,1.07140024848292))
REPRESENTATION_ITEM('')
);
#144=(
BOUNDED_CURVE()
B_SPLINE_CURVE(2,(#5370,#5371,#5372),.UNSPECIFIED.,.F.,.F.)
B_SPLINE_CURVE_WITH_KNOTS((3,3),(0.14973948338295,0.97160236658079),
 .UNSPECIFIED.)
CURVE()
GEOMETRIC_REPRESENTATION_ITEM()
RATIONAL_B_SPLINE_CURVE((1.07140024848292,1.23714644374248,1.07140024848292))
REPRESENTATION_ITEM('')
);
#145=(
BOUNDED_CURVE()
B_SPLINE_CURVE(2,(#5374,#5375,#5376),.UNSPECIFIED.,.F.,.F.)
B_SPLINE_CURVE_WITH_KNOTS((3,3),(0.14973948338295,0.97160236658079),
 .UNSPECIFIED.)
CURVE()
GEOMETRIC_REPRESENTATION_ITEM()
RATIONAL_B_SPLINE_CURVE((1.07140024848292,1.23714644374248,1.07140024848292))
REPRESENTATION_ITEM('')
);
#146=(
BOUNDED_CURVE()
B_SPLINE_CURVE(2,(#5377,#5378,#5379),.UNSPECIFIED.,.F.,.F.)
B_SPLINE_CURVE_WITH_KNOTS((3,3),(0.14973948338295,0.971602366580789),
 .UNSPECIFIED.)
CURVE()
GEOMETRIC_REPRESENTATION_ITEM()
RATIONAL_B_SPLINE_CURVE((1.07140024848292,1.23714644374248,1.07140024848292))
REPRESENTATION_ITEM('')
);
#147=CONICAL_SURFACE('',#3227,0.576175134594813,1.0471975511966);
#148=CONICAL_SURFACE('',#3337,0.4,0.785398163397448);
#149=CONICAL_SURFACE('',#3341,0.41,0.785398163397448);
#150=CONICAL_SURFACE('',#3345,0.26,0.463647609000806);
#151=CONICAL_SURFACE('',#3416,0.475,0.785398163397448);
#152=CONICAL_SURFACE('',#3424,0.255,0.785398163397449);
#153=CONICAL_SURFACE('',#3483,0.734027674973257,1.0471975511966);
#154=CONICAL_SURFACE('',#3485,0.734027674973257,1.0471975511966);
#155=SHAPE_REPRESENTATION_RELATIONSHIP('SRR','None',#5536,#172);
#156=SHAPE_REPRESENTATION_RELATIONSHIP('SRR','None',#5537,#173);
#157=SHAPE_REPRESENTATION_RELATIONSHIP('SRR','None',#5538,#174);
#158=SHAPE_REPRESENTATION_RELATIONSHIP('SRR','None',#5540,#175);
#159=SHAPE_REPRESENTATION_RELATIONSHIP('SRR','None',#5541,#176);
#160=SHAPE_REPRESENTATION_RELATIONSHIP('SRR','None',#5542,#177);
#161=SHAPE_REPRESENTATION_RELATIONSHIP('SRR','None',#5543,#178);
#162=SHAPE_REPRESENTATION_RELATIONSHIP('SRR','None',#5544,#179);
#163=SHAPE_REPRESENTATION_RELATIONSHIP('SRR','None',#5546,#180);
#164=SHAPE_REPRESENTATION_RELATIONSHIP('SRR','None',#5548,#181);
#165=SHAPE_REPRESENTATION_RELATIONSHIP('SRR','None',#5549,#182);
#166=SHAPE_REPRESENTATION_RELATIONSHIP('SRR','None',#5550,#183);
#167=SHAPE_REPRESENTATION_RELATIONSHIP('SRR','None',#5551,#184);
#168=SHAPE_REPRESENTATION_RELATIONSHIP('SRR','None',#5552,#185);
#169=SHAPE_REPRESENTATION_RELATIONSHIP('SRR','None',#5553,#186);
#170=SHAPE_REPRESENTATION_RELATIONSHIP('SRR','None',#5554,#187);
#171=SHAPE_REPRESENTATION_RELATIONSHIP('SRR','None',#5555,#188);
#172=ADVANCED_BREP_SHAPE_REPRESENTATION('',(#206),#5438);
#173=ADVANCED_BREP_SHAPE_REPRESENTATION('',(#207),#5439);
#174=ADVANCED_BREP_SHAPE_REPRESENTATION('',(#208),#5440);
#175=ADVANCED_BREP_SHAPE_REPRESENTATION('',(#209),#5442);
#176=ADVANCED_BREP_SHAPE_REPRESENTATION('',(#210),#5443);
#177=ADVANCED_BREP_SHAPE_REPRESENTATION('',(#211),#5444);
#178=ADVANCED_BREP_SHAPE_REPRESENTATION('',(#212),#5445);
#179=ADVANCED_BREP_SHAPE_REPRESENTATION('',(#128),#5446);
#180=ADVANCED_BREP_SHAPE_REPRESENTATION('',(#213),#5448);
#181=ADVANCED_BREP_SHAPE_REPRESENTATION('',(#214),#5450);
#182=ADVANCED_BREP_SHAPE_REPRESENTATION('',(#215),#5451);
#183=ADVANCED_BREP_SHAPE_REPRESENTATION('',(#216),#5452);
#184=ADVANCED_BREP_SHAPE_REPRESENTATION('',(#217),#5453);
#185=ADVANCED_BREP_SHAPE_REPRESENTATION('',(#218),#5454);
#186=ADVANCED_BREP_SHAPE_REPRESENTATION('',(#219),#5455);
#187=ADVANCED_BREP_SHAPE_REPRESENTATION('',(#220),#5456);
#188=ADVANCED_BREP_SHAPE_REPRESENTATION('',(#221),#5457);
#189=STYLED_ITEM('',(#5696),#206);
#190=STYLED_ITEM('',(#5724),#207);
#191=STYLED_ITEM('',(#5731),#208);
#192=STYLED_ITEM('',(#5710),#209);
#193=STYLED_ITEM('',(#5710),#210);
#194=STYLED_ITEM('',(#5703),#211);
#195=STYLED_ITEM('',(#5710),#212);
#196=STYLED_ITEM('',(#5724),#128);
#197=STYLED_ITEM('',(#5703),#213);
#198=STYLED_ITEM('',(#5731),#214);
#199=STYLED_ITEM('',(#5710),#215);
#200=STYLED_ITEM('',(#5717),#216);
#201=STYLED_ITEM('',(#5724),#217);
#202=STYLED_ITEM('',(#5717),#218);
#203=STYLED_ITEM('',(#5731),#219);
#204=STYLED_ITEM('',(#5724),#220);
#205=STYLED_ITEM('',(#5724),#221);
#206=MANIFOLD_SOLID_BREP('Body1',#2970);
#207=MANIFOLD_SOLID_BREP('Body1',#2971);
#208=MANIFOLD_SOLID_BREP('Body1',#2972);
#209=MANIFOLD_SOLID_BREP('Body1',#2973);
#210=MANIFOLD_SOLID_BREP('Body1',#2974);
#211=MANIFOLD_SOLID_BREP('Body1',#2975);
#212=MANIFOLD_SOLID_BREP('Body1',#2976);
#213=MANIFOLD_SOLID_BREP('Body1',#2979);
#214=MANIFOLD_SOLID_BREP('Body1',#2980);
#215=MANIFOLD_SOLID_BREP('Body1',#2981);
#216=MANIFOLD_SOLID_BREP('Body1',#2982);
#217=MANIFOLD_SOLID_BREP('Body1',#2983);
#218=MANIFOLD_SOLID_BREP('Body1',#2984);
#219=MANIFOLD_SOLID_BREP('Body1',#2985);
#220=MANIFOLD_SOLID_BREP('Body1',#2986);
#221=MANIFOLD_SOLID_BREP('Body1',#2987);
#222=FACE_BOUND('',#577,.T.);
#223=FACE_BOUND('',#579,.T.);
#224=FACE_BOUND('',#584,.T.);
#225=FACE_BOUND('',#589,.T.);
#226=FACE_BOUND('',#591,.T.);
#227=FACE_BOUND('',#596,.T.);
#228=FACE_BOUND('',#602,.T.);
#229=FACE_BOUND('',#603,.T.);
#230=FACE_BOUND('',#604,.T.);
#231=FACE_BOUND('',#605,.T.);
#232=FACE_BOUND('',#606,.T.);
#233=FACE_BOUND('',#607,.T.);
#234=FACE_BOUND('',#609,.T.);
#235=FACE_BOUND('',#610,.T.);
#236=FACE_BOUND('',#622,.T.);
#237=FACE_BOUND('',#641,.T.);
#238=FACE_BOUND('',#642,.T.);
#239=FACE_BOUND('',#643,.T.);
#240=FACE_BOUND('',#644,.T.);
#241=FACE_BOUND('',#646,.T.);
#242=FACE_BOUND('',#647,.T.);
#243=FACE_BOUND('',#653,.T.);
#244=FACE_BOUND('',#654,.T.);
#245=FACE_BOUND('',#655,.T.);
#246=FACE_BOUND('',#660,.T.);
#247=FACE_BOUND('',#661,.T.);
#248=FACE_BOUND('',#662,.T.);
#249=FACE_BOUND('',#670,.T.);
#250=FACE_BOUND('',#672,.T.);
#251=FACE_BOUND('',#676,.T.);
#252=FACE_BOUND('',#678,.T.);
#253=FACE_BOUND('',#683,.T.);
#254=FACE_BOUND('',#699,.T.);
#255=FACE_BOUND('',#707,.T.);
#256=FACE_BOUND('',#708,.T.);
#257=FACE_BOUND('',#712,.T.);
#258=FACE_BOUND('',#713,.T.);
#259=FACE_BOUND('',#719,.T.);
#260=FACE_BOUND('',#720,.T.);
#261=FACE_BOUND('',#721,.T.);
#262=FACE_BOUND('',#727,.T.);
#263=FACE_BOUND('',#728,.T.);
#264=FACE_BOUND('',#729,.T.);
#265=FACE_BOUND('',#733,.T.);
#266=FACE_BOUND('',#740,.T.);
#267=FACE_BOUND('',#746,.T.);
#268=FACE_BOUND('',#748,.T.);
#269=FACE_BOUND('',#754,.T.);
#270=FACE_BOUND('',#756,.T.);
#271=FACE_BOUND('',#762,.T.);
#272=FACE_BOUND('',#764,.T.);
#273=FACE_BOUND('',#766,.T.);
#274=FACE_BOUND('',#779,.T.);
#275=FACE_BOUND('',#781,.T.);
#276=FACE_BOUND('',#792,.T.);
#277=FACE_BOUND('',#794,.T.);
#278=PLANE('',#3182);
#279=PLANE('',#3183);
#280=PLANE('',#3184);
#281=PLANE('',#3188);
#282=PLANE('',#3198);
#283=PLANE('',#3199);
#284=PLANE('',#3200);
#285=PLANE('',#3201);
#286=PLANE('',#3202);
#287=PLANE('',#3206);
#288=PLANE('',#3207);
#289=PLANE('',#3208);
#290=PLANE('',#3209);
#291=PLANE('',#3210);
#292=PLANE('',#3211);
#293=PLANE('',#3212);
#294=PLANE('',#3213);
#295=PLANE('',#3214);
#296=PLANE('',#3215);
#297=PLANE('',#3216);
#298=PLANE('',#3217);
#299=PLANE('',#3218);
#300=PLANE('',#3219);
#301=PLANE('',#3220);
#302=PLANE('',#3221);
#303=PLANE('',#3223);
#304=PLANE('',#3229);
#305=PLANE('',#3230);
#306=PLANE('',#3231);
#307=PLANE('',#3232);
#308=PLANE('',#3233);
#309=PLANE('',#3234);
#310=PLANE('',#3235);
#311=PLANE('',#3236);
#312=PLANE('',#3244);
#313=PLANE('',#3252);
#314=PLANE('',#3253);
#315=PLANE('',#3254);
#316=PLANE('',#3255);
#317=PLANE('',#3256);
#318=PLANE('',#3257);
#319=PLANE('',#3258);
#320=PLANE('',#3259);
#321=PLANE('',#3260);
#322=PLANE('',#3261);
#323=PLANE('',#3262);
#324=PLANE('',#3263);
#325=PLANE('',#3264);
#326=PLANE('',#3265);
#327=PLANE('',#3266);
#328=PLANE('',#3281);
#329=PLANE('',#3285);
#330=PLANE('',#3290);
#331=PLANE('',#3292);
#332=PLANE('',#3293);
#333=PLANE('',#3294);
#334=PLANE('',#3303);
#335=PLANE('',#3304);
#336=PLANE('',#3312);
#337=PLANE('',#3313);
#338=PLANE('',#3318);
#339=PLANE('',#3322);
#340=PLANE('',#3323);
#341=PLANE('',#3325);
#342=PLANE('',#3326);
#343=PLANE('',#3327);
#344=PLANE('',#3328);
#345=PLANE('',#3329);
#346=PLANE('',#3330);
#347=PLANE('',#3331);
#348=PLANE('',#3332);
#349=PLANE('',#3333);
#350=PLANE('',#3335);
#351=PLANE('',#3343);
#352=PLANE('',#3359);
#353=PLANE('',#3360);
#354=PLANE('',#3362);
#355=PLANE('',#3365);
#356=PLANE('',#3372);
#357=PLANE('',#3379);
#358=PLANE('',#3381);
#359=PLANE('',#3382);
#360=PLANE('',#3383);
#361=PLANE('',#3384);
#362=PLANE('',#3385);
#363=PLANE('',#3392);
#364=PLANE('',#3393);
#365=PLANE('',#3394);
#366=PLANE('',#3395);
#367=PLANE('',#3396);
#368=PLANE('',#3397);
#369=PLANE('',#3399);
#370=PLANE('',#3400);
#371=PLANE('',#3410);
#372=PLANE('',#3411);
#373=PLANE('',#3414);
#374=PLANE('',#3420);
#375=PLANE('',#3426);
#376=PLANE('',#3434);
#377=PLANE('',#3435);
#378=PLANE('',#3444);
#379=PLANE('',#3446);
#380=PLANE('',#3450);
#381=PLANE('',#3471);
#382=PLANE('',#3472);
#383=PLANE('',#3480);
#384=PLANE('',#3481);
#385=PLANE('',#3487);
#386=PLANE('',#3488);
#387=PLANE('',#3489);
#388=PLANE('',#3493);
#389=PLANE('',#3494);
#390=PLANE('',#3495);
#391=PLANE('',#3496);
#392=PLANE('',#3497);
#393=FACE_OUTER_BOUND('',#566,.T.);
#394=FACE_OUTER_BOUND('',#567,.T.);
#395=FACE_OUTER_BOUND('',#568,.T.);
#396=FACE_OUTER_BOUND('',#569,.T.);
#397=FACE_OUTER_BOUND('',#570,.T.);
#398=FACE_OUTER_BOUND('',#571,.T.);
#399=FACE_OUTER_BOUND('',#572,.T.);
#400=FACE_OUTER_BOUND('',#573,.T.);
#401=FACE_OUTER_BOUND('',#574,.T.);
#402=FACE_OUTER_BOUND('',#575,.T.);
#403=FACE_OUTER_BOUND('',#576,.T.);
#404=FACE_OUTER_BOUND('',#578,.T.);
#405=FACE_OUTER_BOUND('',#580,.T.);
#406=FACE_OUTER_BOUND('',#581,.T.);
#407=FACE_OUTER_BOUND('',#582,.T.);
#408=FACE_OUTER_BOUND('',#583,.T.);
#409=FACE_OUTER_BOUND('',#585,.T.);
#410=FACE_OUTER_BOUND('',#586,.T.);
#411=FACE_OUTER_BOUND('',#587,.T.);
#412=FACE_OUTER_BOUND('',#588,.T.);
#413=FACE_OUTER_BOUND('',#590,.T.);
#414=FACE_OUTER_BOUND('',#592,.T.);
#415=FACE_OUTER_BOUND('',#593,.T.);
#416=FACE_OUTER_BOUND('',#594,.T.);
#417=FACE_OUTER_BOUND('',#595,.T.);
#418=FACE_OUTER_BOUND('',#597,.T.);
#419=FACE_OUTER_BOUND('',#598,.T.);
#420=FACE_OUTER_BOUND('',#599,.T.);
#421=FACE_OUTER_BOUND('',#600,.T.);
#422=FACE_OUTER_BOUND('',#601,.T.);
#423=FACE_OUTER_BOUND('',#608,.T.);
#424=FACE_OUTER_BOUND('',#611,.T.);
#425=FACE_OUTER_BOUND('',#612,.T.);
#426=FACE_OUTER_BOUND('',#613,.T.);
#427=FACE_OUTER_BOUND('',#614,.T.);
#428=FACE_OUTER_BOUND('',#615,.T.);
#429=FACE_OUTER_BOUND('',#616,.T.);
#430=FACE_OUTER_BOUND('',#617,.T.);
#431=FACE_OUTER_BOUND('',#618,.T.);
#432=FACE_OUTER_BOUND('',#619,.T.);
#433=FACE_OUTER_BOUND('',#620,.T.);
#434=FACE_OUTER_BOUND('',#621,.T.);
#435=FACE_OUTER_BOUND('',#623,.T.);
#436=FACE_OUTER_BOUND('',#624,.T.);
#437=FACE_OUTER_BOUND('',#625,.T.);
#438=FACE_OUTER_BOUND('',#626,.T.);
#439=FACE_OUTER_BOUND('',#627,.T.);
#440=FACE_OUTER_BOUND('',#628,.T.);
#441=FACE_OUTER_BOUND('',#629,.T.);
#442=FACE_OUTER_BOUND('',#630,.T.);
#443=FACE_OUTER_BOUND('',#631,.T.);
#444=FACE_OUTER_BOUND('',#632,.T.);
#445=FACE_OUTER_BOUND('',#633,.T.);
#446=FACE_OUTER_BOUND('',#634,.T.);
#447=FACE_OUTER_BOUND('',#635,.T.);
#448=FACE_OUTER_BOUND('',#636,.T.);
#449=FACE_OUTER_BOUND('',#637,.T.);
#450=FACE_OUTER_BOUND('',#638,.T.);
#451=FACE_OUTER_BOUND('',#639,.T.);
#452=FACE_OUTER_BOUND('',#640,.T.);
#453=FACE_OUTER_BOUND('',#645,.T.);
#454=FACE_OUTER_BOUND('',#648,.T.);
#455=FACE_OUTER_BOUND('',#649,.T.);
#456=FACE_OUTER_BOUND('',#650,.T.);
#457=FACE_OUTER_BOUND('',#651,.T.);
#458=FACE_OUTER_BOUND('',#652,.T.);
#459=FACE_OUTER_BOUND('',#656,.T.);
#460=FACE_OUTER_BOUND('',#657,.T.);
#461=FACE_OUTER_BOUND('',#658,.T.);
#462=FACE_OUTER_BOUND('',#659,.T.);
#463=FACE_OUTER_BOUND('',#663,.T.);
#464=FACE_OUTER_BOUND('',#664,.T.);
#465=FACE_OUTER_BOUND('',#665,.T.);
#466=FACE_OUTER_BOUND('',#666,.T.);
#467=FACE_OUTER_BOUND('',#667,.T.);
#468=FACE_OUTER_BOUND('',#668,.T.);
#469=FACE_OUTER_BOUND('',#669,.T.);
#470=FACE_OUTER_BOUND('',#671,.T.);
#471=FACE_OUTER_BOUND('',#673,.T.);
#472=FACE_OUTER_BOUND('',#674,.T.);
#473=FACE_OUTER_BOUND('',#675,.T.);
#474=FACE_OUTER_BOUND('',#677,.T.);
#475=FACE_OUTER_BOUND('',#679,.T.);
#476=FACE_OUTER_BOUND('',#680,.T.);
#477=FACE_OUTER_BOUND('',#681,.T.);
#478=FACE_OUTER_BOUND('',#682,.T.);
#479=FACE_OUTER_BOUND('',#684,.T.);
#480=FACE_OUTER_BOUND('',#685,.T.);
#481=FACE_OUTER_BOUND('',#686,.T.);
#482=FACE_OUTER_BOUND('',#687,.T.);
#483=FACE_OUTER_BOUND('',#688,.T.);
#484=FACE_OUTER_BOUND('',#689,.T.);
#485=FACE_OUTER_BOUND('',#690,.T.);
#486=FACE_OUTER_BOUND('',#691,.T.);
#487=FACE_OUTER_BOUND('',#692,.T.);
#488=FACE_OUTER_BOUND('',#693,.T.);
#489=FACE_OUTER_BOUND('',#694,.T.);
#490=FACE_OUTER_BOUND('',#695,.T.);
#491=FACE_OUTER_BOUND('',#696,.T.);
#492=FACE_OUTER_BOUND('',#697,.T.);
#493=FACE_OUTER_BOUND('',#698,.T.);
#494=FACE_OUTER_BOUND('',#700,.T.);
#495=FACE_OUTER_BOUND('',#701,.T.);
#496=FACE_OUTER_BOUND('',#702,.T.);
#497=FACE_OUTER_BOUND('',#703,.T.);
#498=FACE_OUTER_BOUND('',#704,.T.);
#499=FACE_OUTER_BOUND('',#705,.T.);
#500=FACE_OUTER_BOUND('',#706,.T.);
#501=FACE_OUTER_BOUND('',#709,.T.);
#502=FACE_OUTER_BOUND('',#710,.T.);
#503=FACE_OUTER_BOUND('',#711,.T.);
#504=FACE_OUTER_BOUND('',#714,.T.);
#505=FACE_OUTER_BOUND('',#715,.T.);
#506=FACE_OUTER_BOUND('',#716,.T.);
#507=FACE_OUTER_BOUND('',#717,.T.);
#508=FACE_OUTER_BOUND('',#718,.T.);
#509=FACE_OUTER_BOUND('',#722,.T.);
#510=FACE_OUTER_BOUND('',#723,.T.);
#511=FACE_OUTER_BOUND('',#724,.T.);
#512=FACE_OUTER_BOUND('',#725,.T.);
#513=FACE_OUTER_BOUND('',#726,.T.);
#514=FACE_OUTER_BOUND('',#730,.T.);
#515=FACE_OUTER_BOUND('',#731,.T.);
#516=FACE_OUTER_BOUND('',#732,.T.);
#517=FACE_OUTER_BOUND('',#734,.T.);
#518=FACE_OUTER_BOUND('',#735,.T.);
#519=FACE_OUTER_BOUND('',#736,.T.);
#520=FACE_OUTER_BOUND('',#737,.T.);
#521=FACE_OUTER_BOUND('',#738,.T.);
#522=FACE_OUTER_BOUND('',#739,.T.);
#523=FACE_OUTER_BOUND('',#741,.T.);
#524=FACE_OUTER_BOUND('',#742,.T.);
#525=FACE_OUTER_BOUND('',#743,.T.);
#526=FACE_OUTER_BOUND('',#744,.T.);
#527=FACE_OUTER_BOUND('',#745,.T.);
#528=FACE_OUTER_BOUND('',#747,.T.);
#529=FACE_OUTER_BOUND('',#749,.T.);
#530=FACE_OUTER_BOUND('',#750,.T.);
#531=FACE_OUTER_BOUND('',#751,.T.);
#532=FACE_OUTER_BOUND('',#752,.T.);
#533=FACE_OUTER_BOUND('',#753,.T.);
#534=FACE_OUTER_BOUND('',#755,.T.);
#535=FACE_OUTER_BOUND('',#757,.T.);
#536=FACE_OUTER_BOUND('',#758,.T.);
#537=FACE_OUTER_BOUND('',#759,.T.);
#538=FACE_OUTER_BOUND('',#760,.T.);
#539=FACE_OUTER_BOUND('',#761,.T.);
#540=FACE_OUTER_BOUND('',#763,.T.);
#541=FACE_OUTER_BOUND('',#765,.T.);
#542=FACE_OUTER_BOUND('',#767,.T.);
#543=FACE_OUTER_BOUND('',#768,.T.);
#544=FACE_OUTER_BOUND('',#769,.T.);
#545=FACE_OUTER_BOUND('',#770,.T.);
#546=FACE_OUTER_BOUND('',#771,.T.);
#547=FACE_OUTER_BOUND('',#772,.T.);
#548=FACE_OUTER_BOUND('',#773,.T.);
#549=FACE_OUTER_BOUND('',#774,.T.);
#550=FACE_OUTER_BOUND('',#775,.T.);
#551=FACE_OUTER_BOUND('',#776,.T.);
#552=FACE_OUTER_BOUND('',#777,.T.);
#553=FACE_OUTER_BOUND('',#778,.T.);
#554=FACE_OUTER_BOUND('',#780,.T.);
#555=FACE_OUTER_BOUND('',#782,.T.);
#556=FACE_OUTER_BOUND('',#783,.T.);
#557=FACE_OUTER_BOUND('',#784,.T.);
#558=FACE_OUTER_BOUND('',#785,.T.);
#559=FACE_OUTER_BOUND('',#786,.T.);
#560=FACE_OUTER_BOUND('',#787,.T.);
#561=FACE_OUTER_BOUND('',#788,.T.);
#562=FACE_OUTER_BOUND('',#789,.T.);
#563=FACE_OUTER_BOUND('',#790,.T.);
#564=FACE_OUTER_BOUND('',#791,.T.);
#565=FACE_OUTER_BOUND('',#793,.T.);
#566=EDGE_LOOP('',(#2001,#2002,#2003,#2004));
#567=EDGE_LOOP('',(#2005,#2006,#2007,#2008));
#568=EDGE_LOOP('',(#2009,#2010,#2011,#2012));
#569=EDGE_LOOP('',(#2013,#2014,#2015,#2016));
#570=EDGE_LOOP('',(#2017,#2018,#2019,#2020));
#571=EDGE_LOOP('',(#2021,#2022,#2023,#2024));
#572=EDGE_LOOP('',(#2025,#2026,#2027,#2028));
#573=EDGE_LOOP('',(#2029,#2030,#2031,#2032));
#574=EDGE_LOOP('',(#2033,#2034,#2035,#2036));
#575=EDGE_LOOP('',(#2037,#2038,#2039,#2040));
#576=EDGE_LOOP('',(#2041,#2042,#2043,#2044));
#577=EDGE_LOOP('',(#2045));
#578=EDGE_LOOP('',(#2046,#2047,#2048,#2049));
#579=EDGE_LOOP('',(#2050));
#580=EDGE_LOOP('',(#2051,#2052,#2053,#2054));
#581=EDGE_LOOP('',(#2055,#2056,#2057,#2058));
#582=EDGE_LOOP('',(#2059,#2060,#2061,#2062));
#583=EDGE_LOOP('',(#2063,#2064,#2065,#2066));
#584=EDGE_LOOP('',(#2067));
#585=EDGE_LOOP('',(#2068,#2069,#2070,#2071));
#586=EDGE_LOOP('',(#2072,#2073,#2074,#2075));
#587=EDGE_LOOP('',(#2076,#2077,#2078,#2079));
#588=EDGE_LOOP('',(#2080,#2081,#2082,#2083));
#589=EDGE_LOOP('',(#2084));
#590=EDGE_LOOP('',(#2085,#2086,#2087,#2088));
#591=EDGE_LOOP('',(#2089));
#592=EDGE_LOOP('',(#2090,#2091,#2092,#2093));
#593=EDGE_LOOP('',(#2094,#2095,#2096,#2097));
#594=EDGE_LOOP('',(#2098,#2099,#2100,#2101));
#595=EDGE_LOOP('',(#2102,#2103,#2104,#2105));
#596=EDGE_LOOP('',(#2106));
#597=EDGE_LOOP('',(#2107,#2108,#2109,#2110));
#598=EDGE_LOOP('',(#2111,#2112,#2113,#2114));
#599=EDGE_LOOP('',(#2115,#2116,#2117,#2118));
#600=EDGE_LOOP('',(#2119,#2120,#2121,#2122));
#601=EDGE_LOOP('',(#2123,#2124,#2125,#2126));
#602=EDGE_LOOP('',(#2127,#2128,#2129,#2130));
#603=EDGE_LOOP('',(#2131));
#604=EDGE_LOOP('',(#2132));
#605=EDGE_LOOP('',(#2133,#2134,#2135,#2136));
#606=EDGE_LOOP('',(#2137,#2138,#2139,#2140));
#607=EDGE_LOOP('',(#2141,#2142,#2143,#2144));
#608=EDGE_LOOP('',(#2145,#2146,#2147,#2148));
#609=EDGE_LOOP('',(#2149));
#610=EDGE_LOOP('',(#2150));
#611=EDGE_LOOP('',(#2151));
#612=EDGE_LOOP('',(#2152,#2153,#2154,#2155));
#613=EDGE_LOOP('',(#2156,#2157,#2158,#2159,#2160,#2161,#2162,#2163,#2164));
#614=EDGE_LOOP('',(#2165,#2166,#2167,#2168));
#615=EDGE_LOOP('',(#2169,#2170,#2171,#2172));
#616=EDGE_LOOP('',(#2173,#2174,#2175,#2176));
#617=EDGE_LOOP('',(#2177,#2178,#2179,#2180));
#618=EDGE_LOOP('',(#2181,#2182,#2183,#2184));
#619=EDGE_LOOP('',(#2185,#2186,#2187,#2188));
#620=EDGE_LOOP('',(#2189));
#621=EDGE_LOOP('',(#2190,#2191,#2192,#2193,#2194,#2195));
#622=EDGE_LOOP('',(#2196));
#623=EDGE_LOOP('',(#2197,#2198,#2199,#2200));
#624=EDGE_LOOP('',(#2201,#2202,#2203,#2204));
#625=EDGE_LOOP('',(#2205,#2206,#2207,#2208,#2209));
#626=EDGE_LOOP('',(#2210,#2211,#2212,#2213,#2214,#2215,#2216,#2217,#2218,
#2219,#2220,#2221));
#627=EDGE_LOOP('',(#2222,#2223,#2224,#2225,#2226,#2227));
#628=EDGE_LOOP('',(#2228,#2229,#2230,#2231));
#629=EDGE_LOOP('',(#2232,#2233,#2234,#2235));
#630=EDGE_LOOP('',(#2236,#2237,#2238,#2239));
#631=EDGE_LOOP('',(#2240,#2241,#2242,#2243,#2244));
#632=EDGE_LOOP('',(#2245,#2246,#2247,#2248));
#633=EDGE_LOOP('',(#2249,#2250,#2251,#2252,#2253,#2254));
#634=EDGE_LOOP('',(#2255,#2256,#2257,#2258));
#635=EDGE_LOOP('',(#2259,#2260,#2261,#2262));
#636=EDGE_LOOP('',(#2263,#2264,#2265,#2266));
#637=EDGE_LOOP('',(#2267,#2268,#2269,#2270));
#638=EDGE_LOOP('',(#2271,#2272,#2273,#2274));
#639=EDGE_LOOP('',(#2275,#2276,#2277,#2278));
#640=EDGE_LOOP('',(#2279,#2280,#2281,#2282));
#641=EDGE_LOOP('',(#2283));
#642=EDGE_LOOP('',(#2284));
#643=EDGE_LOOP('',(#2285,#2286,#2287,#2288));
#644=EDGE_LOOP('',(#2289,#2290,#2291,#2292));
#645=EDGE_LOOP('',(#2293,#2294,#2295,#2296));
#646=EDGE_LOOP('',(#2297));
#647=EDGE_LOOP('',(#2298));
#648=EDGE_LOOP('',(#2299,#2300,#2301,#2302));
#649=EDGE_LOOP('',(#2303,#2304,#2305,#2306));
#650=EDGE_LOOP('',(#2307,#2308,#2309,#2310));
#651=EDGE_LOOP('',(#2311,#2312,#2313,#2314));
#652=EDGE_LOOP('',(#2315,#2316,#2317,#2318,#2319,#2320,#2321,#2322));
#653=EDGE_LOOP('',(#2323));
#654=EDGE_LOOP('',(#2324));
#655=EDGE_LOOP('',(#2325));
#656=EDGE_LOOP('',(#2326,#2327,#2328,#2329));
#657=EDGE_LOOP('',(#2330,#2331,#2332,#2333));
#658=EDGE_LOOP('',(#2334,#2335,#2336,#2337));
#659=EDGE_LOOP('',(#2338,#2339,#2340,#2341,#2342,#2343,#2344,#2345));
#660=EDGE_LOOP('',(#2346));
#661=EDGE_LOOP('',(#2347));
#662=EDGE_LOOP('',(#2348));
#663=EDGE_LOOP('',(#2349,#2350,#2351,#2352));
#664=EDGE_LOOP('',(#2353,#2354,#2355,#2356));
#665=EDGE_LOOP('',(#2357,#2358,#2359,#2360));
#666=EDGE_LOOP('',(#2361,#2362,#2363,#2364));
#667=EDGE_LOOP('',(#2365,#2366,#2367,#2368));
#668=EDGE_LOOP('',(#2369,#2370,#2371,#2372));
#669=EDGE_LOOP('',(#2373));
#670=EDGE_LOOP('',(#2374));
#671=EDGE_LOOP('',(#2375));
#672=EDGE_LOOP('',(#2376));
#673=EDGE_LOOP('',(#2377,#2378,#2379,#2380));
#674=EDGE_LOOP('',(#2381,#2382,#2383,#2384));
#675=EDGE_LOOP('',(#2385));
#676=EDGE_LOOP('',(#2386));
#677=EDGE_LOOP('',(#2387));
#678=EDGE_LOOP('',(#2388));
#679=EDGE_LOOP('',(#2389,#2390,#2391,#2392));
#680=EDGE_LOOP('',(#2393));
#681=EDGE_LOOP('',(#2394,#2395,#2396,#2397));
#682=EDGE_LOOP('',(#2398));
#683=EDGE_LOOP('',(#2399));
#684=EDGE_LOOP('',(#2400));
#685=EDGE_LOOP('',(#2401,#2402,#2403,#2404));
#686=EDGE_LOOP('',(#2405,#2406,#2407,#2408));
#687=EDGE_LOOP('',(#2409,#2410,#2411,#2412));
#688=EDGE_LOOP('',(#2413,#2414,#2415,#2416));
#689=EDGE_LOOP('',(#2417,#2418,#2419,#2420));
#690=EDGE_LOOP('',(#2421,#2422,#2423,#2424));
#691=EDGE_LOOP('',(#2425,#2426,#2427,#2428,#2429,#2430));
#692=EDGE_LOOP('',(#2431,#2432,#2433,#2434,#2435,#2436));
#693=EDGE_LOOP('',(#2437));
#694=EDGE_LOOP('',(#2438));
#695=EDGE_LOOP('',(#2439,#2440,#2441,#2442));
#696=EDGE_LOOP('',(#2443,#2444,#2445,#2446));
#697=EDGE_LOOP('',(#2447,#2448,#2449,#2450));
#698=EDGE_LOOP('',(#2451));
#699=EDGE_LOOP('',(#2452));
#700=EDGE_LOOP('',(#2453,#2454,#2455,#2456));
#701=EDGE_LOOP('',(#2457,#2458,#2459,#2460));
#702=EDGE_LOOP('',(#2461,#2462,#2463,#2464));
#703=EDGE_LOOP('',(#2465,#2466,#2467,#2468));
#704=EDGE_LOOP('',(#2469,#2470,#2471,#2472));
#705=EDGE_LOOP('',(#2473,#2474,#2475,#2476));
#706=EDGE_LOOP('',(#2477,#2478,#2479,#2480));
#707=EDGE_LOOP('',(#2481));
#708=EDGE_LOOP('',(#2482));
#709=EDGE_LOOP('',(#2483,#2484,#2485,#2486));
#710=EDGE_LOOP('',(#2487,#2488,#2489,#2490));
#711=EDGE_LOOP('',(#2491,#2492,#2493,#2494));
#712=EDGE_LOOP('',(#2495));
#713=EDGE_LOOP('',(#2496));
#714=EDGE_LOOP('',(#2497,#2498,#2499,#2500));
#715=EDGE_LOOP('',(#2501));
#716=EDGE_LOOP('',(#2502,#2503,#2504,#2505));
#717=EDGE_LOOP('',(#2506,#2507,#2508,#2509));
#718=EDGE_LOOP('',(#2510,#2511,#2512,#2513));
#719=EDGE_LOOP('',(#2514));
#720=EDGE_LOOP('',(#2515));
#721=EDGE_LOOP('',(#2516));
#722=EDGE_LOOP('',(#2517,#2518,#2519,#2520));
#723=EDGE_LOOP('',(#2521,#2522,#2523,#2524));
#724=EDGE_LOOP('',(#2525,#2526,#2527,#2528));
#725=EDGE_LOOP('',(#2529,#2530,#2531,#2532));
#726=EDGE_LOOP('',(#2533,#2534,#2535,#2536));
#727=EDGE_LOOP('',(#2537));
#728=EDGE_LOOP('',(#2538));
#729=EDGE_LOOP('',(#2539));
#730=EDGE_LOOP('',(#2540,#2541,#2542,#2543));
#731=EDGE_LOOP('',(#2544,#2545,#2546,#2547));
#732=EDGE_LOOP('',(#2548,#2549,#2550,#2551));
#733=EDGE_LOOP('',(#2552));
#734=EDGE_LOOP('',(#2553,#2554,#2555,#2556));
#735=EDGE_LOOP('',(#2557,#2558,#2559,#2560));
#736=EDGE_LOOP('',(#2561,#2562,#2563,#2564,#2565,#2566));
#737=EDGE_LOOP('',(#2567,#2568,#2569,#2570,#2571,#2572));
#738=EDGE_LOOP('',(#2573,#2574,#2575,#2576));
#739=EDGE_LOOP('',(#2577,#2578,#2579,#2580));
#740=EDGE_LOOP('',(#2581));
#741=EDGE_LOOP('',(#2582,#2583));
#742=EDGE_LOOP('',(#2584,#2585,#2586,#2587,#2588));
#743=EDGE_LOOP('',(#2589,#2590,#2591,#2592));
#744=EDGE_LOOP('',(#2593,#2594,#2595,#2596));
#745=EDGE_LOOP('',(#2597));
#746=EDGE_LOOP('',(#2598));
#747=EDGE_LOOP('',(#2599));
#748=EDGE_LOOP('',(#2600));
#749=EDGE_LOOP('',(#2601,#2602,#2603,#2604,#2605,#2606));
#750=EDGE_LOOP('',(#2607));
#751=EDGE_LOOP('',(#2608,#2609,#2610,#2611));
#752=EDGE_LOOP('',(#2612,#2613,#2614,#2615));
#753=EDGE_LOOP('',(#2616));
#754=EDGE_LOOP('',(#2617));
#755=EDGE_LOOP('',(#2618,#2619,#2620,#2621,#2622,#2623,#2624,#2625,#2626));
#756=EDGE_LOOP('',(#2627));
#757=EDGE_LOOP('',(#2628,#2629,#2630,#2631));
#758=EDGE_LOOP('',(#2632));
#759=EDGE_LOOP('',(#2633,#2634,#2635,#2636));
#760=EDGE_LOOP('',(#2637,#2638,#2639,#2640));
#761=EDGE_LOOP('',(#2641));
#762=EDGE_LOOP('',(#2642));
#763=EDGE_LOOP('',(#2643));
#764=EDGE_LOOP('',(#2644));
#765=EDGE_LOOP('',(#2645,#2646,#2647,#2648));
#766=EDGE_LOOP('',(#2649,#2650));
#767=EDGE_LOOP('',(#2651,#2652));
#768=EDGE_LOOP('',(#2653,#2654,#2655,#2656));
#769=EDGE_LOOP('',(#2657,#2658,#2659,#2660,#2661,#2662,#2663,#2664,#2665));
#770=EDGE_LOOP('',(#2666,#2667,#2668));
#771=EDGE_LOOP('',(#2669,#2670,#2671,#2672,#2673));
#772=EDGE_LOOP('',(#2674,#2675,#2676,#2677,#2678,#2679));
#773=EDGE_LOOP('',(#2680,#2681,#2682,#2683,#2684));
#774=EDGE_LOOP('',(#2685));
#775=EDGE_LOOP('',(#2686));
#776=EDGE_LOOP('',(#2687,#2688,#2689,#2690));
#777=EDGE_LOOP('',(#2691,#2692,#2693,#2694));
#778=EDGE_LOOP('',(#2695));
#779=EDGE_LOOP('',(#2696));
#780=EDGE_LOOP('',(#2697));
#781=EDGE_LOOP('',(#2698));
#782=EDGE_LOOP('',(#2699,#2700,#2701,#2702,#2703,#2704,#2705,#2706,#2707));
#783=EDGE_LOOP('',(#2708,#2709,#2710,#2711,#2712,#2713,#2714,#2715,#2716));
#784=EDGE_LOOP('',(#2717,#2718,#2719,#2720));
#785=EDGE_LOOP('',(#2721,#2722,#2723,#2724));
#786=EDGE_LOOP('',(#2725,#2726,#2727,#2728));
#787=EDGE_LOOP('',(#2729,#2730,#2731,#2732));
#788=EDGE_LOOP('',(#2733,#2734,#2735,#2736));
#789=EDGE_LOOP('',(#2737,#2738,#2739,#2740));
#790=EDGE_LOOP('',(#2741,#2742,#2743,#2744));
#791=EDGE_LOOP('',(#2745));
#792=EDGE_LOOP('',(#2746));
#793=EDGE_LOOP('',(#2747));
#794=EDGE_LOOP('',(#2748));
#795=LINE('',#4425,#1032);
#796=LINE('',#4430,#1033);
#797=LINE('',#4432,#1034);
#798=LINE('',#4434,#1035);
#799=LINE('',#4435,#1036);
#800=LINE('',#4439,#1037);
#801=LINE('',#4441,#1038);
#802=LINE('',#4443,#1039);
#803=LINE('',#4444,#1040);
#804=LINE('',#4447,#1041);
#805=LINE('',#4451,#1042);
#806=LINE('',#4456,#1043);
#807=LINE('',#4462,#1044);
#808=LINE('',#4468,#1045);
#809=LINE('',#4473,#1046);
#810=LINE('',#4475,#1047);
#811=LINE('',#4477,#1048);
#812=LINE('',#4478,#1049);
#813=LINE('',#4481,#1050);
#814=LINE('',#4483,#1051);
#815=LINE('',#4484,#1052);
#816=LINE('',#4487,#1053);
#817=LINE('',#4489,#1054);
#818=LINE('',#4490,#1055);
#819=LINE('',#4492,#1056);
#820=LINE('',#4494,#1057);
#821=LINE('',#4499,#1058);
#822=LINE('',#4504,#1059);
#823=LINE('',#4506,#1060);
#824=LINE('',#4508,#1061);
#825=LINE('',#4509,#1062);
#826=LINE('',#4512,#1063);
#827=LINE('',#4514,#1064);
#828=LINE('',#4515,#1065);
#829=LINE('',#4518,#1066);
#830=LINE('',#4520,#1067);
#831=LINE('',#4521,#1068);
#832=LINE('',#4523,#1069);
#833=LINE('',#4525,#1070);
#834=LINE('',#4529,#1071);
#835=LINE('',#4531,#1072);
#836=LINE('',#4533,#1073);
#837=LINE('',#4534,#1074);
#838=LINE('',#4537,#1075);
#839=LINE('',#4539,#1076);
#840=LINE('',#4540,#1077);
#841=LINE('',#4543,#1078);
#842=LINE('',#4545,#1079);
#843=LINE('',#4546,#1080);
#844=LINE('',#4548,#1081);
#845=LINE('',#4550,#1082);
#846=LINE('',#4554,#1083);
#847=LINE('',#4556,#1084);
#848=LINE('',#4558,#1085);
#849=LINE('',#4559,#1086);
#850=LINE('',#4562,#1087);
#851=LINE('',#4564,#1088);
#852=LINE('',#4565,#1089);
#853=LINE('',#4568,#1090);
#854=LINE('',#4570,#1091);
#855=LINE('',#4571,#1092);
#856=LINE('',#4573,#1093);
#857=LINE('',#4574,#1094);
#858=LINE('',#4583,#1095);
#859=LINE('',#4589,#1096);
#860=LINE('',#4615,#1097);
#861=LINE('',#4617,#1098);
#862=LINE('',#4618,#1099);
#863=LINE('',#4621,#1100);
#864=LINE('',#4622,#1101);
#865=LINE('',#4625,#1102);
#866=LINE('',#4626,#1103);
#867=LINE('',#4629,#1104);
#868=LINE('',#4630,#1105);
#869=LINE('',#4633,#1106);
#870=LINE('',#4634,#1107);
#871=LINE('',#4636,#1108);
#872=LINE('',#4644,#1109);
#873=LINE('',#4650,#1110);
#874=LINE('',#4657,#1111);
#875=LINE('',#4659,#1112);
#876=LINE('',#4661,#1113);
#877=LINE('',#4662,#1114);
#878=LINE('',#4665,#1115);
#879=LINE('',#4667,#1116);
#880=LINE('',#4671,#1117);
#881=LINE('',#4675,#1118);
#882=LINE('',#4679,#1119);
#883=LINE('',#4684,#1120);
#884=LINE('',#4686,#1121);
#885=LINE('',#4688,#1122);
#886=LINE('',#4689,#1123);
#887=LINE('',#4691,#1124);
#888=LINE('',#4693,#1125);
#889=LINE('',#4695,#1126);
#890=LINE('',#4698,#1127);
#891=LINE('',#4700,#1128);
#892=LINE('',#4702,#1129);
#893=LINE('',#4703,#1130);
#894=LINE('',#4706,#1131);
#895=LINE('',#4707,#1132);
#896=LINE('',#4710,#1133);
#897=LINE('',#4712,#1134);
#898=LINE('',#4713,#1135);
#899=LINE('',#4715,#1136);
#900=LINE('',#4717,#1137);
#901=LINE('',#4721,#1138);
#902=LINE('',#4723,#1139);
#903=LINE('',#4725,#1140);
#904=LINE('',#4726,#1141);
#905=LINE('',#4729,#1142);
#906=LINE('',#4731,#1143);
#907=LINE('',#4732,#1144);
#908=LINE('',#4735,#1145);
#909=LINE('',#4737,#1146);
#910=LINE('',#4738,#1147);
#911=LINE('',#4740,#1148);
#912=LINE('',#4741,#1149);
#913=LINE('',#4750,#1150);
#914=LINE('',#4756,#1151);
#915=LINE('',#4762,#1152);
#916=LINE('',#4767,#1153);
#917=LINE('',#4771,#1154);
#918=LINE('',#4775,#1155);
#919=LINE('',#4779,#1156);
#920=LINE('',#4783,#1157);
#921=LINE('',#4786,#1158);
#922=LINE('',#4789,#1159);
#923=LINE('',#4790,#1160);
#924=LINE('',#4794,#1161);
#925=LINE('',#4797,#1162);
#926=LINE('',#4799,#1163);
#927=LINE('',#4802,#1164);
#928=LINE('',#4804,#1165);
#929=LINE('',#4807,#1166);
#930=LINE('',#4809,#1167);
#931=LINE('',#4811,#1168);
#932=LINE('',#4819,#1169);
#933=LINE('',#4825,#1170);
#934=LINE('',#4834,#1171);
#935=LINE('',#4840,#1172);
#936=LINE('',#4849,#1173);
#937=LINE('',#4856,#1174);
#938=LINE('',#4864,#1175);
#939=LINE('',#4866,#1176);
#940=LINE('',#4868,#1177);
#941=LINE('',#4869,#1178);
#942=LINE('',#4872,#1179);
#943=LINE('',#4874,#1180);
#944=LINE('',#4875,#1181);
#945=LINE('',#4878,#1182);
#946=LINE('',#4880,#1183);
#947=LINE('',#4881,#1184);
#948=LINE('',#4884,#1185);
#949=LINE('',#4886,#1186);
#950=LINE('',#4887,#1187);
#951=LINE('',#4890,#1188);
#952=LINE('',#4892,#1189);
#953=LINE('',#4893,#1190);
#954=LINE('',#4895,#1191);
#955=LINE('',#4896,#1192);
#956=LINE('',#4908,#1193);
#957=LINE('',#4912,#1194);
#958=LINE('',#4916,#1195);
#959=LINE('',#4923,#1196);
#960=LINE('',#4925,#1197);
#961=LINE('',#4932,#1198);
#962=LINE('',#4938,#1199);
#963=LINE('',#4943,#1200);
#964=LINE('',#4947,#1201);
#965=LINE('',#4951,#1202);
#966=LINE('',#4953,#1203);
#967=LINE('',#4954,#1204);
#968=LINE('',#4957,#1205);
#969=LINE('',#4961,#1206);
#970=LINE('',#4962,#1207);
#971=LINE('',#4973,#1208);
#972=LINE('',#4980,#1209);
#973=LINE('',#4986,#1210);
#974=LINE('',#4991,#1211);
#975=LINE('',#4993,#1212);
#976=LINE('',#4995,#1213);
#977=LINE('',#4996,#1214);
#978=LINE('',#5001,#1215);
#979=LINE('',#5003,#1216);
#980=LINE('',#5004,#1217);
#981=LINE('',#5007,#1218);
#982=LINE('',#5008,#1219);
#983=LINE('',#5011,#1220);
#984=LINE('',#5012,#1221);
#985=LINE('',#5014,#1222);
#986=LINE('',#5020,#1223);
#987=LINE('',#5025,#1224);
#988=LINE('',#5029,#1225);
#989=LINE('',#5033,#1226);
#990=LINE('',#5035,#1227);
#991=LINE('',#5036,#1228);
#992=LINE('',#5039,#1229);
#993=LINE('',#5041,#1230);
#994=LINE('',#5042,#1231);
#995=LINE('',#5045,#1232);
#996=LINE('',#5047,#1233);
#997=LINE('',#5048,#1234);
#998=LINE('',#5051,#1235);
#999=LINE('',#5052,#1236);
#1000=LINE('',#5055,#1237);
#1001=LINE('',#5056,#1238);
#1002=LINE('',#5058,#1239);
#1003=LINE('',#5064,#1240);
#1004=LINE('',#5070,#1241);
#1005=LINE('',#5076,#1242);
#1006=LINE('',#5095,#1243);
#1007=LINE('',#5165,#1244);
#1008=LINE('',#5169,#1245);
#1009=LINE('',#5176,#1246);
#1010=LINE('',#5177,#1247);
#1011=LINE('',#5181,#1248);
#1012=LINE('',#5188,#1249);
#1013=LINE('',#5194,#1250);
#1014=LINE('',#5265,#1251);
#1015=LINE('',#5268,#1252);
#1016=LINE('',#5270,#1253);
#1017=LINE('',#5271,#1254);
#1018=LINE('',#5275,#1255);
#1019=LINE('',#5292,#1256);
#1020=LINE('',#5304,#1257);
#1021=LINE('',#5313,#1258);
#1022=LINE('',#5319,#1259);
#1023=LINE('',#5335,#1260);
#1024=LINE('',#5356,#1261);
#1025=LINE('',#5381,#1262);
#1026=LINE('',#5382,#1263);
#1027=LINE('',#5384,#1264);
#1028=LINE('',#5386,#1265);
#1029=LINE('',#5391,#1266);
#1030=LINE('',#5394,#1267);
#1031=LINE('',#5396,#1268);
#1032=VECTOR('',#3521,0.25);
#1033=VECTOR('',#3526,1.);
#1034=VECTOR('',#3527,1.);
#1035=VECTOR('',#3528,1.);
#1036=VECTOR('',#3529,1.);
#1037=VECTOR('',#3532,1.);
#1038=VECTOR('',#3533,1.);
#1039=VECTOR('',#3534,1.);
#1040=VECTOR('',#3535,1.);
#1041=VECTOR('',#3540,1.);
#1042=VECTOR('',#3547,1.);
#1043=VECTOR('',#3552,0.275);
#1044=VECTOR('',#3559,0.275);
#1045=VECTOR('',#3566,0.61);
#1046=VECTOR('',#3571,1.);
#1047=VECTOR('',#3572,1.);
#1048=VECTOR('',#3573,1.);
#1049=VECTOR('',#3574,1.);
#1050=VECTOR('',#3577,1.);
#1051=VECTOR('',#3578,1.);
#1052=VECTOR('',#3579,1.);
#1053=VECTOR('',#3582,1.);
#1054=VECTOR('',#3583,1.);
#1055=VECTOR('',#3584,1.);
#1056=VECTOR('',#3587,1.);
#1057=VECTOR('',#3590,1.);
#1058=VECTOR('',#3595,0.31);
#1059=VECTOR('',#3600,1.);
#1060=VECTOR('',#3601,1.);
#1061=VECTOR('',#3602,1.);
#1062=VECTOR('',#3603,1.);
#1063=VECTOR('',#3606,1.);
#1064=VECTOR('',#3607,1.);
#1065=VECTOR('',#3608,1.);
#1066=VECTOR('',#3611,1.);
#1067=VECTOR('',#3612,1.);
#1068=VECTOR('',#3613,1.);
#1069=VECTOR('',#3616,1.);
#1070=VECTOR('',#3619,1.);
#1071=VECTOR('',#3622,1.);
#1072=VECTOR('',#3623,1.);
#1073=VECTOR('',#3624,1.);
#1074=VECTOR('',#3625,1.);
#1075=VECTOR('',#3628,1.);
#1076=VECTOR('',#3629,1.);
#1077=VECTOR('',#3630,1.);
#1078=VECTOR('',#3633,1.);
#1079=VECTOR('',#3634,1.);
#1080=VECTOR('',#3635,1.);
#1081=VECTOR('',#3638,1.);
#1082=VECTOR('',#3641,1.);
#1083=VECTOR('',#3644,1.);
#1084=VECTOR('',#3645,1.);
#1085=VECTOR('',#3646,1.);
#1086=VECTOR('',#3647,1.);
#1087=VECTOR('',#3650,1.);
#1088=VECTOR('',#3651,1.);
#1089=VECTOR('',#3652,1.);
#1090=VECTOR('',#3655,1.);
#1091=VECTOR('',#3656,1.);
#1092=VECTOR('',#3657,1.);
#1093=VECTOR('',#3660,1.);
#1094=VECTOR('',#3661,1.);
#1095=VECTOR('',#3674,0.3);
#1096=VECTOR('',#3681,0.576175134594813);
#1097=VECTOR('',#3684,1.);
#1098=VECTOR('',#3685,1.);
#1099=VECTOR('',#3686,1.);
#1100=VECTOR('',#3689,1.);
#1101=VECTOR('',#3690,1.);
#1102=VECTOR('',#3693,1.);
#1103=VECTOR('',#3694,1.);
#1104=VECTOR('',#3697,1.);
#1105=VECTOR('',#3698,1.);
#1106=VECTOR('',#3701,1.);
#1107=VECTOR('',#3702,1.);
#1108=VECTOR('',#3705,1.);
#1109=VECTOR('',#3716,0.275);
#1110=VECTOR('',#3723,0.274999999999999);
#1111=VECTOR('',#3730,1.);
#1112=VECTOR('',#3731,1.);
#1113=VECTOR('',#3732,1.);
#1114=VECTOR('',#3733,1.);
#1115=VECTOR('',#3736,1.);
#1116=VECTOR('',#3737,1.);
#1117=VECTOR('',#3740,0.300000000000001);
#1118=VECTOR('',#3743,1.);
#1119=VECTOR('',#3746,1.);
#1120=VECTOR('',#3753,1.);
#1121=VECTOR('',#3754,1.);
#1122=VECTOR('',#3755,1.);
#1123=VECTOR('',#3756,1.);
#1124=VECTOR('',#3759,1.);
#1125=VECTOR('',#3762,1.);
#1126=VECTOR('',#3765,1.);
#1127=VECTOR('',#3768,1.);
#1128=VECTOR('',#3769,1.);
#1129=VECTOR('',#3770,1.);
#1130=VECTOR('',#3771,1.);
#1131=VECTOR('',#3774,1.);
#1132=VECTOR('',#3775,1.);
#1133=VECTOR('',#3778,1.);
#1134=VECTOR('',#3779,1.);
#1135=VECTOR('',#3780,1.);
#1136=VECTOR('',#3783,1.);
#1137=VECTOR('',#3786,1.);
#1138=VECTOR('',#3789,1.);
#1139=VECTOR('',#3790,1.);
#1140=VECTOR('',#3791,1.);
#1141=VECTOR('',#3792,1.);
#1142=VECTOR('',#3795,1.);
#1143=VECTOR('',#3796,1.);
#1144=VECTOR('',#3797,1.);
#1145=VECTOR('',#3800,1.);
#1146=VECTOR('',#3801,1.);
#1147=VECTOR('',#3802,1.);
#1148=VECTOR('',#3805,1.);
#1149=VECTOR('',#3806,1.);
#1150=VECTOR('',#3819,0.275);
#1151=VECTOR('',#3826,0.31);
#1152=VECTOR('',#3833,0.31);
#1153=VECTOR('',#3838,1.);
#1154=VECTOR('',#3841,1.);
#1155=VECTOR('',#3846,1.);
#1156=VECTOR('',#3849,1.);
#1157=VECTOR('',#3852,1.);
#1158=VECTOR('',#3855,1.);
#1159=VECTOR('',#3858,1.);
#1160=VECTOR('',#3859,1.);
#1161=VECTOR('',#3864,1.);
#1162=VECTOR('',#3867,1.);
#1163=VECTOR('',#3868,1.);
#1164=VECTOR('',#3873,1.);
#1165=VECTOR('',#3874,1.);
#1166=VECTOR('',#3877,1.);
#1167=VECTOR('',#3880,1.);
#1168=VECTOR('',#3883,1.);
#1169=VECTOR('',#3894,0.31);
#1170=VECTOR('',#3901,0.4);
#1171=VECTOR('',#3914,0.31);
#1172=VECTOR('',#3921,0.4);
#1173=VECTOR('',#3934,0.21);
#1174=VECTOR('',#3943,0.7);
#1175=VECTOR('',#3954,1.);
#1176=VECTOR('',#3955,1.);
#1177=VECTOR('',#3956,1.);
#1178=VECTOR('',#3957,1.);
#1179=VECTOR('',#3960,1.);
#1180=VECTOR('',#3961,1.);
#1181=VECTOR('',#3962,1.);
#1182=VECTOR('',#3965,1.);
#1183=VECTOR('',#3966,1.);
#1184=VECTOR('',#3967,1.);
#1185=VECTOR('',#3970,1.);
#1186=VECTOR('',#3971,1.);
#1187=VECTOR('',#3972,1.);
#1188=VECTOR('',#3975,1.);
#1189=VECTOR('',#3976,1.);
#1190=VECTOR('',#3977,1.);
#1191=VECTOR('',#3980,1.);
#1192=VECTOR('',#3981,1.);
#1193=VECTOR('',#3998,0.4);
#1194=VECTOR('',#4003,0.425);
#1195=VECTOR('',#4008,0.41);
#1196=VECTOR('',#4017,0.26);
#1197=VECTOR('',#4020,0.25);
#1198=VECTOR('',#4029,0.31);
#1199=VECTOR('',#4036,0.31);
#1200=VECTOR('',#4041,1.);
#1201=VECTOR('',#4044,1.);
#1202=VECTOR('',#4049,1.);
#1203=VECTOR('',#4050,1.);
#1204=VECTOR('',#4051,1.);
#1205=VECTOR('',#4054,1.);
#1206=VECTOR('',#4059,1.);
#1207=VECTOR('',#4060,1.);
#1208=VECTOR('',#4077,0.34);
#1209=VECTOR('',#4086,0.425);
#1210=VECTOR('',#4093,0.425);
#1211=VECTOR('',#4098,1.);
#1212=VECTOR('',#4099,1.);
#1213=VECTOR('',#4100,1.);
#1214=VECTOR('',#4101,1.);
#1215=VECTOR('',#4106,1.);
#1216=VECTOR('',#4107,1.);
#1217=VECTOR('',#4108,1.);
#1218=VECTOR('',#4111,1.);
#1219=VECTOR('',#4112,1.);
#1220=VECTOR('',#4115,1.);
#1221=VECTOR('',#4116,1.);
#1222=VECTOR('',#4119,1.);
#1223=VECTOR('',#4126,0.31);
#1224=VECTOR('',#4131,1.);
#1225=VECTOR('',#4134,1.);
#1226=VECTOR('',#4139,1.);
#1227=VECTOR('',#4140,1.);
#1228=VECTOR('',#4141,1.);
#1229=VECTOR('',#4144,1.);
#1230=VECTOR('',#4145,1.);
#1231=VECTOR('',#4146,1.);
#1232=VECTOR('',#4149,1.);
#1233=VECTOR('',#4150,1.);
#1234=VECTOR('',#4151,1.);
#1235=VECTOR('',#4154,1.);
#1236=VECTOR('',#4155,1.);
#1237=VECTOR('',#4158,1.);
#1238=VECTOR('',#4159,1.);
#1239=VECTOR('',#4162,1.);
#1240=VECTOR('',#4173,0.6);
#1241=VECTOR('',#4180,0.31);
#1242=VECTOR('',#4187,0.4);
#1243=VECTOR('',#4198,0.08);
#1244=VECTOR('',#4207,0.475);
#1245=VECTOR('',#4212,0.5);
#1246=VECTOR('',#4221,0.3);
#1247=VECTOR('',#4222,0.3);
#1248=VECTOR('',#4227,0.255);
#1249=VECTOR('',#4236,0.32);
#1250=VECTOR('',#4243,0.6);
#1251=VECTOR('',#4270,1.);
#1252=VECTOR('',#4273,1.);
#1253=VECTOR('',#4274,1.);
#1254=VECTOR('',#4275,1.);
#1255=VECTOR('',#4280,0.08);
#1256=VECTOR('',#4309,0.4);
#1257=VECTOR('',#4324,0.4);
#1258=VECTOR('',#4337,0.42);
#1259=VECTOR('',#4344,0.8);
#1260=VECTOR('',#4355,0.734027674973257);
#1261=VECTOR('',#4362,0.734027674973257);
#1262=VECTOR('',#4365,1.);
#1263=VECTOR('',#4366,1.);
#1264=VECTOR('',#4369,1.);
#1265=VECTOR('',#4372,1.);
#1266=VECTOR('',#4377,0.4);
#1267=VECTOR('',#4382,1.);
#1268=VECTOR('',#4385,1.);
#1269=CIRCLE('',#3180,0.25);
#1270=CIRCLE('',#3181,0.25);
#1271=CIRCLE('',#3185,0.3);
#1272=CIRCLE('',#3187,0.3);
#1273=CIRCLE('',#3190,0.275);
#1274=CIRCLE('',#3191,0.275);
#1275=CIRCLE('',#3193,0.275);
#1276=CIRCLE('',#3194,0.275);
#1277=CIRCLE('',#3196,0.61);
#1278=CIRCLE('',#3197,0.61);
#1279=CIRCLE('',#3204,0.31);
#1280=CIRCLE('',#3205,0.31);
#1281=CIRCLE('',#3224,0.2942);
#1282=CIRCLE('',#3226,0.2942);
#1283=CIRCLE('',#3228,0.475);
#1284=CIRCLE('',#3239,0.275);
#1285=CIRCLE('',#3240,0.275);
#1286=CIRCLE('',#3242,0.274999999999999);
#1287=CIRCLE('',#3243,0.274999999999999);
#1288=CIRCLE('',#3245,0.300000000000001);
#1289=CIRCLE('',#3247,0.300000000000001);
#1290=CIRCLE('',#3248,0.300000000000001);
#1291=CIRCLE('',#3249,0.300000000000001);
#1292=CIRCLE('',#3250,0.300000000000001);
#1293=CIRCLE('',#3251,0.300000000000001);
#1294=CIRCLE('',#3270,0.275);
#1295=CIRCLE('',#3271,0.275);
#1296=CIRCLE('',#3273,0.31);
#1297=CIRCLE('',#3274,0.31);
#1298=CIRCLE('',#3276,0.31);
#1299=CIRCLE('',#3277,0.31);
#1300=CIRCLE('',#3279,0.6);
#1301=CIRCLE('',#3280,0.6);
#1302=CIRCLE('',#3282,0.6);
#1303=CIRCLE('',#3283,0.6);
#1304=CIRCLE('',#3284,0.6);
#1305=CIRCLE('',#3287,0.6);
#1306=CIRCLE('',#3289,0.6);
#1307=CIRCLE('',#3291,0.6);
#1308=CIRCLE('',#3298,0.31);
#1309=CIRCLE('',#3299,0.31);
#1310=CIRCLE('',#3301,0.4);
#1311=CIRCLE('',#3302,0.4);
#1312=CIRCLE('',#3307,0.31);
#1313=CIRCLE('',#3308,0.31);
#1314=CIRCLE('',#3310,0.4);
#1315=CIRCLE('',#3311,0.4);
#1316=CIRCLE('',#3316,0.21);
#1317=CIRCLE('',#3317,0.21);
#1318=CIRCLE('',#3320,0.7);
#1319=CIRCLE('',#3321,0.7);
#1320=CIRCLE('',#3334,0.24505);
#1321=CIRCLE('',#3336,0.375);
#1322=CIRCLE('',#3338,0.425);
#1323=CIRCLE('',#3340,0.425);
#1324=CIRCLE('',#3342,0.395);
#1325=CIRCLE('',#3344,0.27);
#1326=CIRCLE('',#3346,0.24505);
#1327=CIRCLE('',#3351,0.31);
#1328=CIRCLE('',#3352,0.31);
#1329=CIRCLE('',#3354,0.31);
#1330=CIRCLE('',#3355,0.31);
#1331=CIRCLE('',#3357,0.6);
#1332=CIRCLE('',#3358,0.6);
#1333=CIRCLE('',#3361,0.6);
#1334=CIRCLE('',#3364,0.6);
#1335=CIRCLE('',#3370,0.34);
#1336=CIRCLE('',#3371,0.34);
#1337=CIRCLE('',#3374,0.425);
#1338=CIRCLE('',#3375,0.425);
#1339=CIRCLE('',#3377,0.425);
#1340=CIRCLE('',#3378,0.425);
#1341=CIRCLE('',#3380,0.6);
#1342=CIRCLE('',#3387,0.31);
#1343=CIRCLE('',#3388,0.31);
#1344=CIRCLE('',#3390,0.6);
#1345=CIRCLE('',#3391,0.6);
#1346=CIRCLE('',#3398,0.6);
#1347=CIRCLE('',#3401,0.6);
#1348=CIRCLE('',#3405,0.31);
#1349=CIRCLE('',#3406,0.31);
#1350=CIRCLE('',#3408,0.4);
#1351=CIRCLE('',#3409,0.4);
#1352=CIRCLE('',#3415,0.45);
#1353=CIRCLE('',#3417,0.5);
#1354=CIRCLE('',#3419,0.5);
#1355=CIRCLE('',#3421,0.3);
#1356=CIRCLE('',#3423,0.3);
#1357=CIRCLE('',#3425,0.21);
#1358=CIRCLE('',#3429,0.32);
#1359=CIRCLE('',#3430,0.32);
#1360=CIRCLE('',#3432,0.6);
#1361=CIRCLE('',#3433,0.6);
#1362=CIRCLE('',#3442,0.08);
#1363=CIRCLE('',#3443,0.04);
#1364=CIRCLE('',#3445,0.08);
#1365=CIRCLE('',#3448,0.08);
#1366=CIRCLE('',#3449,0.08);
#1367=CIRCLE('',#3462,0.4);
#1368=CIRCLE('',#3463,0.4);
#1369=CIRCLE('',#3464,0.4);
#1370=CIRCLE('',#3466,0.6);
#1371=CIRCLE('',#3467,0.4);
#1372=CIRCLE('',#3468,0.4);
#1373=CIRCLE('',#3470,0.4);
#1374=CIRCLE('',#3475,0.42);
#1375=CIRCLE('',#3476,0.42);
#1376=CIRCLE('',#3478,0.8);
#1377=CIRCLE('',#3479,0.8);
#1378=CIRCLE('',#3484,0.6175);
#1379=CIRCLE('',#3486,0.6175);
#1380=CIRCLE('',#3491,0.338975);
#1381=CIRCLE('',#3492,0.338975);
#1382=VERTEX_POINT('',#4422);
#1383=VERTEX_POINT('',#4424);
#1384=VERTEX_POINT('',#4428);
#1385=VERTEX_POINT('',#4429);
#1386=VERTEX_POINT('',#4431);
#1387=VERTEX_POINT('',#4433);
#1388=VERTEX_POINT('',#4437);
#1389=VERTEX_POINT('',#4438);
#1390=VERTEX_POINT('',#4440);
#1391=VERTEX_POINT('',#4442);
#1392=VERTEX_POINT('',#4453);
#1393=VERTEX_POINT('',#4455);
#1394=VERTEX_POINT('',#4459);
#1395=VERTEX_POINT('',#4461);
#1396=VERTEX_POINT('',#4465);
#1397=VERTEX_POINT('',#4467);
#1398=VERTEX_POINT('',#4471);
#1399=VERTEX_POINT('',#4472);
#1400=VERTEX_POINT('',#4474);
#1401=VERTEX_POINT('',#4476);
#1402=VERTEX_POINT('',#4480);
#1403=VERTEX_POINT('',#4482);
#1404=VERTEX_POINT('',#4486);
#1405=VERTEX_POINT('',#4488);
#1406=VERTEX_POINT('',#4496);
#1407=VERTEX_POINT('',#4498);
#1408=VERTEX_POINT('',#4502);
#1409=VERTEX_POINT('',#4503);
#1410=VERTEX_POINT('',#4505);
#1411=VERTEX_POINT('',#4507);
#1412=VERTEX_POINT('',#4511);
#1413=VERTEX_POINT('',#4513);
#1414=VERTEX_POINT('',#4517);
#1415=VERTEX_POINT('',#4519);
#1416=VERTEX_POINT('',#4527);
#1417=VERTEX_POINT('',#4528);
#1418=VERTEX_POINT('',#4530);
#1419=VERTEX_POINT('',#4532);
#1420=VERTEX_POINT('',#4536);
#1421=VERTEX_POINT('',#4538);
#1422=VERTEX_POINT('',#4542);
#1423=VERTEX_POINT('',#4544);
#1424=VERTEX_POINT('',#4552);
#1425=VERTEX_POINT('',#4553);
#1426=VERTEX_POINT('',#4555);
#1427=VERTEX_POINT('',#4557);
#1428=VERTEX_POINT('',#4561);
#1429=VERTEX_POINT('',#4563);
#1430=VERTEX_POINT('',#4567);
#1431=VERTEX_POINT('',#4569);
#1432=VERTEX_POINT('',#4579);
#1433=VERTEX_POINT('',#4582);
#1434=VERTEX_POINT('',#4586);
#1435=VERTEX_POINT('',#4588);
#1436=VERTEX_POINT('',#4590);
#1437=VERTEX_POINT('',#4594);
#1438=VERTEX_POINT('',#4598);
#1439=VERTEX_POINT('',#4602);
#1440=VERTEX_POINT('',#4606);
#1441=VERTEX_POINT('',#4614);
#1442=VERTEX_POINT('',#4616);
#1443=VERTEX_POINT('',#4620);
#1444=VERTEX_POINT('',#4624);
#1445=VERTEX_POINT('',#4628);
#1446=VERTEX_POINT('',#4632);
#1447=VERTEX_POINT('',#4641);
#1448=VERTEX_POINT('',#4643);
#1449=VERTEX_POINT('',#4647);
#1450=VERTEX_POINT('',#4649);
#1451=VERTEX_POINT('',#4653);
#1452=VERTEX_POINT('',#4654);
#1453=VERTEX_POINT('',#4656);
#1454=VERTEX_POINT('',#4658);
#1455=VERTEX_POINT('',#4660);
#1456=VERTEX_POINT('',#4664);
#1457=VERTEX_POINT('',#4666);
#1458=VERTEX_POINT('',#4668);
#1459=VERTEX_POINT('',#4670);
#1460=VERTEX_POINT('',#4672);
#1461=VERTEX_POINT('',#4674);
#1462=VERTEX_POINT('',#4676);
#1463=VERTEX_POINT('',#4678);
#1464=VERTEX_POINT('',#4683);
#1465=VERTEX_POINT('',#4685);
#1466=VERTEX_POINT('',#4687);
#1467=VERTEX_POINT('',#4697);
#1468=VERTEX_POINT('',#4699);
#1469=VERTEX_POINT('',#4701);
#1470=VERTEX_POINT('',#4705);
#1471=VERTEX_POINT('',#4709);
#1472=VERTEX_POINT('',#4711);
#1473=VERTEX_POINT('',#4719);
#1474=VERTEX_POINT('',#4720);
#1475=VERTEX_POINT('',#4722);
#1476=VERTEX_POINT('',#4724);
#1477=VERTEX_POINT('',#4728);
#1478=VERTEX_POINT('',#4730);
#1479=VERTEX_POINT('',#4734);
#1480=VERTEX_POINT('',#4736);
#1481=VERTEX_POINT('',#4747);
#1482=VERTEX_POINT('',#4749);
#1483=VERTEX_POINT('',#4753);
#1484=VERTEX_POINT('',#4755);
#1485=VERTEX_POINT('',#4759);
#1486=VERTEX_POINT('',#4761);
#1487=VERTEX_POINT('',#4765);
#1488=VERTEX_POINT('',#4766);
#1489=VERTEX_POINT('',#4768);
#1490=VERTEX_POINT('',#4770);
#1491=VERTEX_POINT('',#4774);
#1492=VERTEX_POINT('',#4776);
#1493=VERTEX_POINT('',#4778);
#1494=VERTEX_POINT('',#4780);
#1495=VERTEX_POINT('',#4782);
#1496=VERTEX_POINT('',#4784);
#1497=VERTEX_POINT('',#4788);
#1498=VERTEX_POINT('',#4792);
#1499=VERTEX_POINT('',#4796);
#1500=VERTEX_POINT('',#4798);
#1501=VERTEX_POINT('',#4803);
#1502=VERTEX_POINT('',#4805);
#1503=VERTEX_POINT('',#4816);
#1504=VERTEX_POINT('',#4818);
#1505=VERTEX_POINT('',#4822);
#1506=VERTEX_POINT('',#4824);
#1507=VERTEX_POINT('',#4831);
#1508=VERTEX_POINT('',#4833);
#1509=VERTEX_POINT('',#4837);
#1510=VERTEX_POINT('',#4839);
#1511=VERTEX_POINT('',#4846);
#1512=VERTEX_POINT('',#4848);
#1513=VERTEX_POINT('',#4853);
#1514=VERTEX_POINT('',#4855);
#1515=VERTEX_POINT('',#4862);
#1516=VERTEX_POINT('',#4863);
#1517=VERTEX_POINT('',#4865);
#1518=VERTEX_POINT('',#4867);
#1519=VERTEX_POINT('',#4871);
#1520=VERTEX_POINT('',#4873);
#1521=VERTEX_POINT('',#4877);
#1522=VERTEX_POINT('',#4879);
#1523=VERTEX_POINT('',#4883);
#1524=VERTEX_POINT('',#4885);
#1525=VERTEX_POINT('',#4889);
#1526=VERTEX_POINT('',#4891);
#1527=VERTEX_POINT('',#4900);
#1528=VERTEX_POINT('',#4903);
#1529=VERTEX_POINT('',#4906);
#1530=VERTEX_POINT('',#4910);
#1531=VERTEX_POINT('',#4914);
#1532=VERTEX_POINT('',#4918);
#1533=VERTEX_POINT('',#4921);
#1534=VERTEX_POINT('',#4929);
#1535=VERTEX_POINT('',#4931);
#1536=VERTEX_POINT('',#4935);
#1537=VERTEX_POINT('',#4937);
#1538=VERTEX_POINT('',#4941);
#1539=VERTEX_POINT('',#4942);
#1540=VERTEX_POINT('',#4944);
#1541=VERTEX_POINT('',#4946);
#1542=VERTEX_POINT('',#4950);
#1543=VERTEX_POINT('',#4952);
#1544=VERTEX_POINT('',#4956);
#1545=VERTEX_POINT('',#4960);
#1546=VERTEX_POINT('',#4970);
#1547=VERTEX_POINT('',#4972);
#1548=VERTEX_POINT('',#4977);
#1549=VERTEX_POINT('',#4979);
#1550=VERTEX_POINT('',#4983);
#1551=VERTEX_POINT('',#4985);
#1552=VERTEX_POINT('',#4989);
#1553=VERTEX_POINT('',#4990);
#1554=VERTEX_POINT('',#4992);
#1555=VERTEX_POINT('',#4994);
#1556=VERTEX_POINT('',#4997);
#1557=VERTEX_POINT('',#5000);
#1558=VERTEX_POINT('',#5002);
#1559=VERTEX_POINT('',#5006);
#1560=VERTEX_POINT('',#5010);
#1561=VERTEX_POINT('',#5017);
#1562=VERTEX_POINT('',#5019);
#1563=VERTEX_POINT('',#5023);
#1564=VERTEX_POINT('',#5024);
#1565=VERTEX_POINT('',#5026);
#1566=VERTEX_POINT('',#5028);
#1567=VERTEX_POINT('',#5032);
#1568=VERTEX_POINT('',#5034);
#1569=VERTEX_POINT('',#5038);
#1570=VERTEX_POINT('',#5040);
#1571=VERTEX_POINT('',#5044);
#1572=VERTEX_POINT('',#5046);
#1573=VERTEX_POINT('',#5050);
#1574=VERTEX_POINT('',#5054);
#1575=VERTEX_POINT('',#5067);
#1576=VERTEX_POINT('',#5069);
#1577=VERTEX_POINT('',#5073);
#1578=VERTEX_POINT('',#5075);
#1579=VERTEX_POINT('',#5082);
#1580=VERTEX_POINT('',#5083);
#1581=VERTEX_POINT('',#5094);
#1582=VERTEX_POINT('',#5130);
#1583=VERTEX_POINT('',#5160);
#1584=VERTEX_POINT('',#5163);
#1585=VERTEX_POINT('',#5167);
#1586=VERTEX_POINT('',#5171);
#1587=VERTEX_POINT('',#5174);
#1588=VERTEX_POINT('',#5179);
#1589=VERTEX_POINT('',#5185);
#1590=VERTEX_POINT('',#5187);
#1591=VERTEX_POINT('',#5191);
#1592=VERTEX_POINT('',#5193);
#1593=VERTEX_POINT('',#5204);
#1594=VERTEX_POINT('',#5207);
#1595=VERTEX_POINT('',#5208);
#1596=VERTEX_POINT('',#5262);
#1597=VERTEX_POINT('',#5263);
#1598=VERTEX_POINT('',#5267);
#1599=VERTEX_POINT('',#5269);
#1600=VERTEX_POINT('',#5273);
#1601=VERTEX_POINT('',#5289);
#1602=VERTEX_POINT('',#5291);
#1603=VERTEX_POINT('',#5293);
#1604=VERTEX_POINT('',#5297);
#1605=VERTEX_POINT('',#5299);
#1606=VERTEX_POINT('',#5303);
#1607=VERTEX_POINT('',#5310);
#1608=VERTEX_POINT('',#5312);
#1609=VERTEX_POINT('',#5316);
#1610=VERTEX_POINT('',#5318);
#1611=VERTEX_POINT('',#5325);
#1612=VERTEX_POINT('',#5326);
#1613=VERTEX_POINT('',#5330);
#1614=VERTEX_POINT('',#5334);
#1615=VERTEX_POINT('',#5337);
#1616=VERTEX_POINT('',#5341);
#1617=VERTEX_POINT('',#5345);
#1618=VERTEX_POINT('',#5353);
#1619=VERTEX_POINT('',#5355);
#1620=VERTEX_POINT('',#5357);
#1621=VERTEX_POINT('',#5361);
#1622=VERTEX_POINT('',#5365);
#1623=VERTEX_POINT('',#5369);
#1624=VERTEX_POINT('',#5373);
#1625=VERTEX_POINT('',#5388);
#1626=VERTEX_POINT('',#5390);
#1627=EDGE_CURVE('',#1382,#1382,#1269,.T.);
#1628=EDGE_CURVE('',#1382,#1383,#795,.T.);
#1629=EDGE_CURVE('',#1383,#1383,#1270,.T.);
#1630=EDGE_CURVE('',#1384,#1385,#796,.T.);
#1631=EDGE_CURVE('',#1386,#1384,#797,.T.);
#1632=EDGE_CURVE('',#1387,#1386,#798,.T.);
#1633=EDGE_CURVE('',#1385,#1387,#799,.T.);
#1634=EDGE_CURVE('',#1388,#1389,#800,.T.);
#1635=EDGE_CURVE('',#1390,#1388,#801,.T.);
#1636=EDGE_CURVE('',#1390,#1391,#802,.T.);
#1637=EDGE_CURVE('',#1389,#1391,#803,.T.);
#1638=EDGE_CURVE('',#1390,#1387,#1271,.T.);
#1639=EDGE_CURVE('',#1385,#1388,#804,.T.);
#1640=EDGE_CURVE('',#1391,#1386,#1272,.T.);
#1641=EDGE_CURVE('',#1389,#1384,#805,.T.);
#1642=EDGE_CURVE('',#1392,#1392,#1273,.T.);
#1643=EDGE_CURVE('',#1392,#1393,#806,.T.);
#1644=EDGE_CURVE('',#1393,#1393,#1274,.T.);
#1645=EDGE_CURVE('',#1394,#1394,#1275,.T.);
#1646=EDGE_CURVE('',#1394,#1395,#807,.T.);
#1647=EDGE_CURVE('',#1395,#1395,#1276,.T.);
#1648=EDGE_CURVE('',#1396,#1396,#1277,.T.);
#1649=EDGE_CURVE('',#1396,#1397,#808,.T.);
#1650=EDGE_CURVE('',#1397,#1397,#1278,.T.);
#1651=EDGE_CURVE('',#1398,#1399,#809,.T.);
#1652=EDGE_CURVE('',#1398,#1400,#810,.T.);
#1653=EDGE_CURVE('',#1400,#1401,#811,.T.);
#1654=EDGE_CURVE('',#1401,#1399,#812,.T.);
#1655=EDGE_CURVE('',#1402,#1398,#813,.T.);
#1656=EDGE_CURVE('',#1403,#1402,#814,.T.);
#1657=EDGE_CURVE('',#1400,#1403,#815,.T.);
#1658=EDGE_CURVE('',#1399,#1404,#816,.T.);
#1659=EDGE_CURVE('',#1401,#1405,#817,.T.);
#1660=EDGE_CURVE('',#1404,#1405,#818,.T.);
#1661=EDGE_CURVE('',#1405,#1403,#819,.T.);
#1662=EDGE_CURVE('',#1404,#1402,#820,.T.);
#1663=EDGE_CURVE('',#1406,#1406,#1279,.T.);
#1664=EDGE_CURVE('',#1406,#1407,#821,.T.);
#1665=EDGE_CURVE('',#1407,#1407,#1280,.T.);
#1666=EDGE_CURVE('',#1408,#1409,#822,.T.);
#1667=EDGE_CURVE('',#1408,#1410,#823,.T.);
#1668=EDGE_CURVE('',#1410,#1411,#824,.T.);
#1669=EDGE_CURVE('',#1411,#1409,#825,.T.);
#1670=EDGE_CURVE('',#1412,#1408,#826,.T.);
#1671=EDGE_CURVE('',#1413,#1412,#827,.T.);
#1672=EDGE_CURVE('',#1410,#1413,#828,.T.);
#1673=EDGE_CURVE('',#1409,#1414,#829,.T.);
#1674=EDGE_CURVE('',#1411,#1415,#830,.T.);
#1675=EDGE_CURVE('',#1414,#1415,#831,.T.);
#1676=EDGE_CURVE('',#1415,#1413,#832,.T.);
#1677=EDGE_CURVE('',#1414,#1412,#833,.T.);
#1678=EDGE_CURVE('',#1416,#1417,#834,.T.);
#1679=EDGE_CURVE('',#1416,#1418,#835,.T.);
#1680=EDGE_CURVE('',#1418,#1419,#836,.T.);
#1681=EDGE_CURVE('',#1419,#1417,#837,.T.);
#1682=EDGE_CURVE('',#1420,#1416,#838,.T.);
#1683=EDGE_CURVE('',#1421,#1420,#839,.T.);
#1684=EDGE_CURVE('',#1418,#1421,#840,.T.);
#1685=EDGE_CURVE('',#1417,#1422,#841,.T.);
#1686=EDGE_CURVE('',#1419,#1423,#842,.T.);
#1687=EDGE_CURVE('',#1422,#1423,#843,.T.);
#1688=EDGE_CURVE('',#1423,#1421,#844,.T.);
#1689=EDGE_CURVE('',#1422,#1420,#845,.T.);
#1690=EDGE_CURVE('',#1424,#1425,#846,.T.);
#1691=EDGE_CURVE('',#1425,#1426,#847,.T.);
#1692=EDGE_CURVE('',#1427,#1426,#848,.T.);
#1693=EDGE_CURVE('',#1424,#1427,#849,.T.);
#1694=EDGE_CURVE('',#1428,#1424,#850,.T.);
#1695=EDGE_CURVE('',#1429,#1427,#851,.T.);
#1696=EDGE_CURVE('',#1428,#1429,#852,.T.);
#1697=EDGE_CURVE('',#1430,#1428,#853,.T.);
#1698=EDGE_CURVE('',#1431,#1429,#854,.T.);
#1699=EDGE_CURVE('',#1430,#1431,#855,.T.);
#1700=EDGE_CURVE('',#1425,#1430,#856,.T.);
#1701=EDGE_CURVE('',#1426,#1431,#857,.T.);
#1702=EDGE_CURVE('',#1432,#1432,#1281,.T.);
#1703=EDGE_CURVE('',#1432,#1433,#858,.T.);
#1704=EDGE_CURVE('',#1433,#1433,#1282,.F.);
#1705=EDGE_CURVE('',#1434,#1434,#1283,.T.);
#1706=EDGE_CURVE('',#1434,#1435,#859,.T.);
#1707=EDGE_CURVE('',#1436,#1435,#129,.T.);
#1708=EDGE_CURVE('',#1437,#1436,#130,.T.);
#1709=EDGE_CURVE('',#1438,#1437,#131,.T.);
#1710=EDGE_CURVE('',#1439,#1438,#132,.T.);
#1711=EDGE_CURVE('',#1440,#1439,#133,.T.);
#1712=EDGE_CURVE('',#1435,#1440,#134,.T.);
#1713=EDGE_CURVE('',#1441,#1439,#860,.T.);
#1714=EDGE_CURVE('',#1441,#1442,#861,.T.);
#1715=EDGE_CURVE('',#1442,#1440,#862,.T.);
#1716=EDGE_CURVE('',#1443,#1438,#863,.T.);
#1717=EDGE_CURVE('',#1443,#1441,#864,.T.);
#1718=EDGE_CURVE('',#1444,#1437,#865,.T.);
#1719=EDGE_CURVE('',#1444,#1443,#866,.T.);
#1720=EDGE_CURVE('',#1445,#1436,#867,.T.);
#1721=EDGE_CURVE('',#1445,#1444,#868,.T.);
#1722=EDGE_CURVE('',#1446,#1435,#869,.T.);
#1723=EDGE_CURVE('',#1446,#1445,#870,.T.);
#1724=EDGE_CURVE('',#1442,#1446,#871,.T.);
#1725=EDGE_CURVE('',#1447,#1447,#1284,.T.);
#1726=EDGE_CURVE('',#1447,#1448,#872,.T.);
#1727=EDGE_CURVE('',#1448,#1448,#1285,.T.);
#1728=EDGE_CURVE('',#1449,#1449,#1286,.T.);
#1729=EDGE_CURVE('',#1449,#1450,#873,.T.);
#1730=EDGE_CURVE('',#1450,#1450,#1287,.T.);
#1731=EDGE_CURVE('',#1451,#1452,#1288,.T.);
#1732=EDGE_CURVE('',#1452,#1453,#874,.T.);
#1733=EDGE_CURVE('',#1454,#1453,#875,.T.);
#1734=EDGE_CURVE('',#1454,#1455,#876,.T.);
#1735=EDGE_CURVE('',#1455,#1451,#877,.T.);
#1736=EDGE_CURVE('',#1452,#1456,#878,.T.);
#1737=EDGE_CURVE('',#1457,#1451,#879,.T.);
#1738=EDGE_CURVE('',#1458,#1457,#1289,.T.);
#1739=EDGE_CURVE('',#1458,#1459,#880,.T.);
#1740=EDGE_CURVE('',#1459,#1460,#1290,.T.);
#1741=EDGE_CURVE('',#1461,#1460,#881,.T.);
#1742=EDGE_CURVE('',#1462,#1461,#1291,.T.);
#1743=EDGE_CURVE('',#1463,#1462,#882,.T.);
#1744=EDGE_CURVE('',#1463,#1459,#1292,.T.);
#1745=EDGE_CURVE('',#1456,#1458,#1293,.T.);
#1746=EDGE_CURVE('',#1457,#1464,#883,.T.);
#1747=EDGE_CURVE('',#1464,#1465,#884,.T.);
#1748=EDGE_CURVE('',#1466,#1465,#885,.T.);
#1749=EDGE_CURVE('',#1466,#1456,#886,.T.);
#1750=EDGE_CURVE('',#1455,#1464,#887,.T.);
#1751=EDGE_CURVE('',#1465,#1454,#888,.T.);
#1752=EDGE_CURVE('',#1453,#1466,#889,.T.);
#1753=EDGE_CURVE('',#1461,#1467,#890,.T.);
#1754=EDGE_CURVE('',#1467,#1468,#891,.T.);
#1755=EDGE_CURVE('',#1469,#1468,#892,.T.);
#1756=EDGE_CURVE('',#1469,#1462,#893,.T.);
#1757=EDGE_CURVE('',#1470,#1460,#894,.T.);
#1758=EDGE_CURVE('',#1470,#1467,#895,.T.);
#1759=EDGE_CURVE('',#1463,#1471,#896,.T.);
#1760=EDGE_CURVE('',#1472,#1471,#897,.T.);
#1761=EDGE_CURVE('',#1472,#1470,#898,.T.);
#1762=EDGE_CURVE('',#1468,#1472,#899,.T.);
#1763=EDGE_CURVE('',#1471,#1469,#900,.T.);
#1764=EDGE_CURVE('',#1473,#1474,#901,.T.);
#1765=EDGE_CURVE('',#1474,#1475,#902,.T.);
#1766=EDGE_CURVE('',#1476,#1475,#903,.T.);
#1767=EDGE_CURVE('',#1473,#1476,#904,.T.);
#1768=EDGE_CURVE('',#1477,#1473,#905,.T.);
#1769=EDGE_CURVE('',#1478,#1476,#906,.T.);
#1770=EDGE_CURVE('',#1477,#1478,#907,.T.);
#1771=EDGE_CURVE('',#1479,#1477,#908,.T.);
#1772=EDGE_CURVE('',#1480,#1478,#909,.T.);
#1773=EDGE_CURVE('',#1479,#1480,#910,.T.);
#1774=EDGE_CURVE('',#1474,#1479,#911,.T.);
#1775=EDGE_CURVE('',#1475,#1480,#912,.T.);
#1776=EDGE_CURVE('',#1481,#1481,#1294,.T.);
#1777=EDGE_CURVE('',#1481,#1482,#913,.T.);
#1778=EDGE_CURVE('',#1482,#1482,#1295,.T.);
#1779=EDGE_CURVE('',#1483,#1483,#1296,.T.);
#1780=EDGE_CURVE('',#1483,#1484,#914,.T.);
#1781=EDGE_CURVE('',#1484,#1484,#1297,.T.);
#1782=EDGE_CURVE('',#1485,#1485,#1298,.T.);
#1783=EDGE_CURVE('',#1485,#1486,#915,.T.);
#1784=EDGE_CURVE('',#1486,#1486,#1299,.T.);
#1785=EDGE_CURVE('',#1487,#1488,#916,.T.);
#1786=EDGE_CURVE('',#1489,#1487,#1300,.T.);
#1787=EDGE_CURVE('',#1490,#1489,#917,.T.);
#1788=EDGE_CURVE('',#1490,#1488,#1301,.T.);
#1789=EDGE_CURVE('',#1491,#1490,#918,.T.);
#1790=EDGE_CURVE('',#1492,#1491,#1302,.T.);
#1791=EDGE_CURVE('',#1493,#1492,#919,.T.);
#1792=EDGE_CURVE('',#1494,#1493,#1303,.T.);
#1793=EDGE_CURVE('',#1495,#1494,#920,.T.);
#1794=EDGE_CURVE('',#1496,#1495,#1304,.T.);
#1795=EDGE_CURVE('',#1488,#1496,#921,.T.);
#1796=EDGE_CURVE('',#1497,#1489,#922,.T.);
#1797=EDGE_CURVE('',#1497,#1491,#923,.T.);
#1798=EDGE_CURVE('',#1498,#1497,#1305,.T.);
#1799=EDGE_CURVE('',#1492,#1498,#924,.T.);
#1800=EDGE_CURVE('',#1496,#1499,#925,.T.);
#1801=EDGE_CURVE('',#1500,#1495,#926,.T.);
#1802=EDGE_CURVE('',#1499,#1500,#1306,.T.);
#1803=EDGE_CURVE('',#1487,#1499,#927,.T.);
#1804=EDGE_CURVE('',#1500,#1501,#928,.T.);
#1805=EDGE_CURVE('',#1501,#1502,#1307,.T.);
#1806=EDGE_CURVE('',#1502,#1498,#929,.T.);
#1807=EDGE_CURVE('',#1501,#1494,#930,.T.);
#1808=EDGE_CURVE('',#1493,#1502,#931,.T.);
#1809=EDGE_CURVE('',#1503,#1503,#1308,.T.);
#1810=EDGE_CURVE('',#1503,#1504,#932,.T.);
#1811=EDGE_CURVE('',#1504,#1504,#1309,.T.);
#1812=EDGE_CURVE('',#1505,#1505,#1310,.T.);
#1813=EDGE_CURVE('',#1505,#1506,#933,.T.);
#1814=EDGE_CURVE('',#1506,#1506,#1311,.T.);
#1815=EDGE_CURVE('',#1507,#1507,#1312,.T.);
#1816=EDGE_CURVE('',#1507,#1508,#934,.T.);
#1817=EDGE_CURVE('',#1508,#1508,#1313,.T.);
#1818=EDGE_CURVE('',#1509,#1509,#1314,.T.);
#1819=EDGE_CURVE('',#1509,#1510,#935,.T.);
#1820=EDGE_CURVE('',#1510,#1510,#1315,.T.);
#1821=EDGE_CURVE('',#1511,#1511,#1316,.T.);
#1822=EDGE_CURVE('',#1511,#1512,#936,.T.);
#1823=EDGE_CURVE('',#1512,#1512,#1317,.T.);
#1824=EDGE_CURVE('',#1513,#1513,#1318,.T.);
#1825=EDGE_CURVE('',#1513,#1514,#937,.T.);
#1826=EDGE_CURVE('',#1514,#1514,#1319,.T.);
#1827=EDGE_CURVE('',#1515,#1516,#938,.T.);
#1828=EDGE_CURVE('',#1516,#1517,#939,.T.);
#1829=EDGE_CURVE('',#1517,#1518,#940,.T.);
#1830=EDGE_CURVE('',#1515,#1518,#941,.T.);
#1831=EDGE_CURVE('',#1516,#1519,#942,.T.);
#1832=EDGE_CURVE('',#1519,#1520,#943,.T.);
#1833=EDGE_CURVE('',#1520,#1517,#944,.T.);
#1834=EDGE_CURVE('',#1519,#1521,#945,.T.);
#1835=EDGE_CURVE('',#1521,#1522,#946,.T.);
#1836=EDGE_CURVE('',#1522,#1520,#947,.T.);
#1837=EDGE_CURVE('',#1521,#1523,#948,.T.);
#1838=EDGE_CURVE('',#1523,#1524,#949,.T.);
#1839=EDGE_CURVE('',#1524,#1522,#950,.T.);
#1840=EDGE_CURVE('',#1523,#1525,#951,.T.);
#1841=EDGE_CURVE('',#1525,#1526,#952,.T.);
#1842=EDGE_CURVE('',#1526,#1524,#953,.T.);
#1843=EDGE_CURVE('',#1525,#1515,#954,.T.);
#1844=EDGE_CURVE('',#1518,#1526,#955,.T.);
#1845=EDGE_CURVE('',#1527,#1527,#1320,.T.);
#1846=EDGE_CURVE('',#1528,#1528,#1321,.T.);
#1847=EDGE_CURVE('',#1529,#1529,#1322,.T.);
#1848=EDGE_CURVE('',#1529,#1528,#956,.T.);
#1849=EDGE_CURVE('',#1530,#1530,#1323,.T.);
#1850=EDGE_CURVE('',#1530,#1529,#957,.T.);
#1851=EDGE_CURVE('',#1531,#1531,#1324,.T.);
#1852=EDGE_CURVE('',#1531,#1530,#958,.T.);
#1853=EDGE_CURVE('',#1532,#1532,#1325,.T.);
#1854=EDGE_CURVE('',#1533,#1533,#1326,.F.);
#1855=EDGE_CURVE('',#1533,#1532,#959,.T.);
#1856=EDGE_CURVE('',#1527,#1533,#960,.T.);
#1857=EDGE_CURVE('',#1534,#1534,#1327,.T.);
#1858=EDGE_CURVE('',#1534,#1535,#961,.T.);
#1859=EDGE_CURVE('',#1535,#1535,#1328,.T.);
#1860=EDGE_CURVE('',#1536,#1536,#1329,.T.);
#1861=EDGE_CURVE('',#1536,#1537,#962,.T.);
#1862=EDGE_CURVE('',#1537,#1537,#1330,.T.);
#1863=EDGE_CURVE('',#1538,#1539,#963,.T.);
#1864=EDGE_CURVE('',#1540,#1538,#1331,.T.);
#1865=EDGE_CURVE('',#1541,#1540,#964,.T.);
#1866=EDGE_CURVE('',#1541,#1539,#1332,.T.);
#1867=EDGE_CURVE('',#1539,#1542,#965,.T.);
#1868=EDGE_CURVE('',#1543,#1542,#966,.T.);
#1869=EDGE_CURVE('',#1538,#1543,#967,.T.);
#1870=EDGE_CURVE('',#1544,#1541,#968,.T.);
#1871=EDGE_CURVE('',#1542,#1544,#1333,.T.);
#1872=EDGE_CURVE('',#1545,#1540,#969,.T.);
#1873=EDGE_CURVE('',#1544,#1545,#970,.T.);
#1874=EDGE_CURVE('',#1543,#1545,#1334,.T.);
#1875=EDGE_CURVE('',#1546,#1546,#1335,.T.);
#1876=EDGE_CURVE('',#1546,#1547,#971,.T.);
#1877=EDGE_CURVE('',#1547,#1547,#1336,.T.);
#1878=EDGE_CURVE('',#1548,#1548,#1337,.T.);
#1879=EDGE_CURVE('',#1548,#1549,#972,.T.);
#1880=EDGE_CURVE('',#1549,#1549,#1338,.T.);
#1881=EDGE_CURVE('',#1550,#1550,#1339,.T.);
#1882=EDGE_CURVE('',#1550,#1551,#973,.T.);
#1883=EDGE_CURVE('',#1551,#1551,#1340,.T.);
#1884=EDGE_CURVE('',#1552,#1553,#974,.T.);
#1885=EDGE_CURVE('',#1554,#1552,#975,.T.);
#1886=EDGE_CURVE('',#1555,#1554,#976,.T.);
#1887=EDGE_CURVE('',#1553,#1555,#977,.T.);
#1888=EDGE_CURVE('',#1556,#1556,#1341,.T.);
#1889=EDGE_CURVE('',#1552,#1557,#978,.T.);
#1890=EDGE_CURVE('',#1558,#1557,#979,.T.);
#1891=EDGE_CURVE('',#1554,#1558,#980,.T.);
#1892=EDGE_CURVE('',#1559,#1558,#981,.T.);
#1893=EDGE_CURVE('',#1555,#1559,#982,.T.);
#1894=EDGE_CURVE('',#1560,#1559,#983,.T.);
#1895=EDGE_CURVE('',#1553,#1560,#984,.T.);
#1896=EDGE_CURVE('',#1557,#1560,#985,.T.);
#1897=EDGE_CURVE('',#1561,#1561,#1342,.T.);
#1898=EDGE_CURVE('',#1561,#1562,#986,.T.);
#1899=EDGE_CURVE('',#1562,#1562,#1343,.T.);
#1900=EDGE_CURVE('',#1563,#1564,#987,.T.);
#1901=EDGE_CURVE('',#1565,#1564,#1344,.T.);
#1902=EDGE_CURVE('',#1566,#1565,#988,.T.);
#1903=EDGE_CURVE('',#1566,#1563,#1345,.T.);
#1904=EDGE_CURVE('',#1566,#1567,#989,.T.);
#1905=EDGE_CURVE('',#1567,#1568,#990,.T.);
#1906=EDGE_CURVE('',#1568,#1563,#991,.T.);
#1907=EDGE_CURVE('',#1569,#1567,#992,.T.);
#1908=EDGE_CURVE('',#1570,#1569,#993,.T.);
#1909=EDGE_CURVE('',#1570,#1568,#994,.T.);
#1910=EDGE_CURVE('',#1571,#1570,#995,.T.);
#1911=EDGE_CURVE('',#1569,#1572,#996,.T.);
#1912=EDGE_CURVE('',#1571,#1572,#997,.T.);
#1913=EDGE_CURVE('',#1573,#1565,#998,.T.);
#1914=EDGE_CURVE('',#1572,#1573,#999,.T.);
#1915=EDGE_CURVE('',#1564,#1574,#1000,.T.);
#1916=EDGE_CURVE('',#1571,#1574,#1001,.T.);
#1917=EDGE_CURVE('',#1574,#1573,#1002,.T.);
#1918=EDGE_CURVE('',#1572,#1571,#1346,.T.);
#1919=EDGE_CURVE('',#1571,#1572,#1347,.T.);
#1920=EDGE_CURVE('',#1556,#1571,#1003,.T.);
#1921=EDGE_CURVE('',#1575,#1575,#1348,.T.);
#1922=EDGE_CURVE('',#1575,#1576,#1004,.T.);
#1923=EDGE_CURVE('',#1576,#1576,#1349,.T.);
#1924=EDGE_CURVE('',#1577,#1577,#1350,.T.);
#1925=EDGE_CURVE('',#1577,#1578,#1005,.T.);
#1926=EDGE_CURVE('',#1578,#1578,#1351,.T.);
#1927=EDGE_CURVE('',#1579,#1580,#13,.T.);
#1928=EDGE_CURVE('',#1579,#1581,#1006,.T.);
#1929=EDGE_CURVE('',#1581,#1581,#14,.T.);
#1930=EDGE_CURVE('',#1582,#1579,#15,.T.);
#1931=EDGE_CURVE('',#1580,#1582,#16,.T.);
#1932=EDGE_CURVE('',#1583,#1583,#1352,.T.);
#1933=EDGE_CURVE('',#1584,#1584,#1353,.T.);
#1934=EDGE_CURVE('',#1584,#1583,#1007,.T.);
#1935=EDGE_CURVE('',#1585,#1585,#1354,.T.);
#1936=EDGE_CURVE('',#1585,#1584,#1008,.T.);
#1937=EDGE_CURVE('',#1586,#1586,#1355,.T.);
#1938=EDGE_CURVE('',#1587,#1587,#1356,.T.);
#1939=EDGE_CURVE('',#1587,#1580,#1009,.T.);
#1940=EDGE_CURVE('',#1582,#1586,#1010,.T.);
#1941=EDGE_CURVE('',#1588,#1588,#1357,.T.);
#1942=EDGE_CURVE('',#1588,#1587,#1011,.T.);
#1943=EDGE_CURVE('',#1589,#1589,#1358,.T.);
#1944=EDGE_CURVE('',#1589,#1590,#1012,.T.);
#1945=EDGE_CURVE('',#1590,#1590,#1359,.T.);
#1946=EDGE_CURVE('',#1591,#1591,#1360,.T.);
#1947=EDGE_CURVE('',#1591,#1592,#1013,.T.);
#1948=EDGE_CURVE('',#1592,#1592,#1361,.T.);
#1949=EDGE_CURVE('',#1593,#1593,#1362,.T.);
#1950=EDGE_CURVE('',#1593,#1593,#1363,.T.);
#1951=EDGE_CURVE('',#1594,#1595,#17,.T.);
#1952=EDGE_CURVE('',#1595,#1594,#18,.T.);
#1953=EDGE_CURVE('',#1596,#1597,#1364,.T.);
#1954=EDGE_CURVE('',#1596,#1597,#1014,.T.);
#1955=EDGE_CURVE('',#1597,#1598,#1015,.T.);
#1956=EDGE_CURVE('',#1599,#1598,#1016,.T.);
#1957=EDGE_CURVE('',#1596,#1599,#1017,.T.);
#1958=EDGE_CURVE('',#1600,#1599,#1365,.T.);
#1959=EDGE_CURVE('',#1600,#1595,#1018,.T.);
#1960=EDGE_CURVE('',#1598,#1600,#1366,.T.);
#1961=EDGE_CURVE('',#1601,#1601,#1367,.T.);
#1962=EDGE_CURVE('',#1601,#1602,#1019,.T.);
#1963=EDGE_CURVE('',#1602,#1603,#1368,.T.);
#1964=EDGE_CURVE('',#1603,#1602,#1369,.T.);
#1965=EDGE_CURVE('',#1603,#1604,#1370,.T.);
#1966=EDGE_CURVE('',#1604,#1605,#1371,.T.);
#1967=EDGE_CURVE('',#1605,#1604,#1372,.T.);
#1968=EDGE_CURVE('',#1605,#1606,#1020,.T.);
#1969=EDGE_CURVE('',#1606,#1606,#1373,.T.);
#1970=EDGE_CURVE('',#1607,#1607,#1374,.T.);
#1971=EDGE_CURVE('',#1607,#1608,#1021,.T.);
#1972=EDGE_CURVE('',#1608,#1608,#1375,.T.);
#1973=EDGE_CURVE('',#1609,#1609,#1376,.T.);
#1974=EDGE_CURVE('',#1609,#1610,#1022,.T.);
#1975=EDGE_CURVE('',#1610,#1610,#1377,.T.);
#1976=EDGE_CURVE('',#1611,#1612,#135,.T.);
#1977=EDGE_CURVE('',#1613,#1611,#136,.T.);
#1978=EDGE_CURVE('',#1613,#1614,#1023,.T.);
#1979=EDGE_CURVE('',#1614,#1614,#1378,.T.);
#1980=EDGE_CURVE('',#1615,#1613,#137,.T.);
#1981=EDGE_CURVE('',#1616,#1615,#138,.T.);
#1982=EDGE_CURVE('',#1617,#1616,#139,.T.);
#1983=EDGE_CURVE('',#1612,#1617,#140,.T.);
#1984=EDGE_CURVE('',#1618,#1618,#1379,.T.);
#1985=EDGE_CURVE('',#1618,#1619,#1024,.T.);
#1986=EDGE_CURVE('',#1620,#1619,#141,.T.);
#1987=EDGE_CURVE('',#1621,#1620,#142,.T.);
#1988=EDGE_CURVE('',#1622,#1621,#143,.T.);
#1989=EDGE_CURVE('',#1623,#1622,#144,.T.);
#1990=EDGE_CURVE('',#1624,#1623,#145,.T.);
#1991=EDGE_CURVE('',#1619,#1624,#146,.T.);
#1992=EDGE_CURVE('',#1615,#1624,#1025,.T.);
#1993=EDGE_CURVE('',#1616,#1623,#1026,.T.);
#1994=EDGE_CURVE('',#1613,#1619,#1027,.T.);
#1995=EDGE_CURVE('',#1611,#1620,#1028,.T.);
#1996=EDGE_CURVE('',#1625,#1625,#1380,.F.);
#1997=EDGE_CURVE('',#1625,#1626,#1029,.T.);
#1998=EDGE_CURVE('',#1626,#1626,#1381,.F.);
#1999=EDGE_CURVE('',#1612,#1621,#1030,.T.);
#2000=EDGE_CURVE('',#1617,#1622,#1031,.T.);
#2001=ORIENTED_EDGE('',*,*,#1627,.F.);
#2002=ORIENTED_EDGE('',*,*,#1628,.T.);
#2003=ORIENTED_EDGE('',*,*,#1629,.T.);
#2004=ORIENTED_EDGE('',*,*,#1628,.F.);
#2005=ORIENTED_EDGE('',*,*,#1630,.F.);
#2006=ORIENTED_EDGE('',*,*,#1631,.F.);
#2007=ORIENTED_EDGE('',*,*,#1632,.F.);
#2008=ORIENTED_EDGE('',*,*,#1633,.F.);
#2009=ORIENTED_EDGE('',*,*,#1634,.F.);
#2010=ORIENTED_EDGE('',*,*,#1635,.F.);
#2011=ORIENTED_EDGE('',*,*,#1636,.T.);
#2012=ORIENTED_EDGE('',*,*,#1637,.F.);
#2013=ORIENTED_EDGE('',*,*,#1638,.F.);
#2014=ORIENTED_EDGE('',*,*,#1635,.T.);
#2015=ORIENTED_EDGE('',*,*,#1639,.F.);
#2016=ORIENTED_EDGE('',*,*,#1633,.T.);
#2017=ORIENTED_EDGE('',*,*,#1636,.F.);
#2018=ORIENTED_EDGE('',*,*,#1638,.T.);
#2019=ORIENTED_EDGE('',*,*,#1632,.T.);
#2020=ORIENTED_EDGE('',*,*,#1640,.F.);
#2021=ORIENTED_EDGE('',*,*,#1640,.T.);
#2022=ORIENTED_EDGE('',*,*,#1631,.T.);
#2023=ORIENTED_EDGE('',*,*,#1641,.F.);
#2024=ORIENTED_EDGE('',*,*,#1637,.T.);
#2025=ORIENTED_EDGE('',*,*,#1642,.F.);
#2026=ORIENTED_EDGE('',*,*,#1643,.T.);
#2027=ORIENTED_EDGE('',*,*,#1644,.F.);
#2028=ORIENTED_EDGE('',*,*,#1643,.F.);
#2029=ORIENTED_EDGE('',*,*,#1645,.F.);
#2030=ORIENTED_EDGE('',*,*,#1646,.T.);
#2031=ORIENTED_EDGE('',*,*,#1647,.F.);
#2032=ORIENTED_EDGE('',*,*,#1646,.F.);
#2033=ORIENTED_EDGE('',*,*,#1648,.F.);
#2034=ORIENTED_EDGE('',*,*,#1649,.T.);
#2035=ORIENTED_EDGE('',*,*,#1650,.F.);
#2036=ORIENTED_EDGE('',*,*,#1649,.F.);
#2037=ORIENTED_EDGE('',*,*,#1651,.F.);
#2038=ORIENTED_EDGE('',*,*,#1652,.T.);
#2039=ORIENTED_EDGE('',*,*,#1653,.T.);
#2040=ORIENTED_EDGE('',*,*,#1654,.T.);
#2041=ORIENTED_EDGE('',*,*,#1655,.F.);
#2042=ORIENTED_EDGE('',*,*,#1656,.F.);
#2043=ORIENTED_EDGE('',*,*,#1657,.F.);
#2044=ORIENTED_EDGE('',*,*,#1652,.F.);
#2045=ORIENTED_EDGE('',*,*,#1650,.T.);
#2046=ORIENTED_EDGE('',*,*,#1658,.F.);
#2047=ORIENTED_EDGE('',*,*,#1654,.F.);
#2048=ORIENTED_EDGE('',*,*,#1659,.T.);
#2049=ORIENTED_EDGE('',*,*,#1660,.F.);
#2050=ORIENTED_EDGE('',*,*,#1648,.T.);
#2051=ORIENTED_EDGE('',*,*,#1653,.F.);
#2052=ORIENTED_EDGE('',*,*,#1657,.T.);
#2053=ORIENTED_EDGE('',*,*,#1661,.F.);
#2054=ORIENTED_EDGE('',*,*,#1659,.F.);
#2055=ORIENTED_EDGE('',*,*,#1662,.F.);
#2056=ORIENTED_EDGE('',*,*,#1660,.T.);
#2057=ORIENTED_EDGE('',*,*,#1661,.T.);
#2058=ORIENTED_EDGE('',*,*,#1656,.T.);
#2059=ORIENTED_EDGE('',*,*,#1663,.F.);
#2060=ORIENTED_EDGE('',*,*,#1664,.T.);
#2061=ORIENTED_EDGE('',*,*,#1665,.F.);
#2062=ORIENTED_EDGE('',*,*,#1664,.F.);
#2063=ORIENTED_EDGE('',*,*,#1666,.F.);
#2064=ORIENTED_EDGE('',*,*,#1667,.T.);
#2065=ORIENTED_EDGE('',*,*,#1668,.T.);
#2066=ORIENTED_EDGE('',*,*,#1669,.T.);
#2067=ORIENTED_EDGE('',*,*,#1629,.F.);
#2068=ORIENTED_EDGE('',*,*,#1670,.F.);
#2069=ORIENTED_EDGE('',*,*,#1671,.F.);
#2070=ORIENTED_EDGE('',*,*,#1672,.F.);
#2071=ORIENTED_EDGE('',*,*,#1667,.F.);
#2072=ORIENTED_EDGE('',*,*,#1673,.F.);
#2073=ORIENTED_EDGE('',*,*,#1669,.F.);
#2074=ORIENTED_EDGE('',*,*,#1674,.T.);
#2075=ORIENTED_EDGE('',*,*,#1675,.F.);
#2076=ORIENTED_EDGE('',*,*,#1668,.F.);
#2077=ORIENTED_EDGE('',*,*,#1672,.T.);
#2078=ORIENTED_EDGE('',*,*,#1676,.F.);
#2079=ORIENTED_EDGE('',*,*,#1674,.F.);
#2080=ORIENTED_EDGE('',*,*,#1677,.F.);
#2081=ORIENTED_EDGE('',*,*,#1675,.T.);
#2082=ORIENTED_EDGE('',*,*,#1676,.T.);
#2083=ORIENTED_EDGE('',*,*,#1671,.T.);
#2084=ORIENTED_EDGE('',*,*,#1627,.T.);
#2085=ORIENTED_EDGE('',*,*,#1678,.F.);
#2086=ORIENTED_EDGE('',*,*,#1679,.T.);
#2087=ORIENTED_EDGE('',*,*,#1680,.T.);
#2088=ORIENTED_EDGE('',*,*,#1681,.T.);
#2089=ORIENTED_EDGE('',*,*,#1663,.T.);
#2090=ORIENTED_EDGE('',*,*,#1682,.F.);
#2091=ORIENTED_EDGE('',*,*,#1683,.F.);
#2092=ORIENTED_EDGE('',*,*,#1684,.F.);
#2093=ORIENTED_EDGE('',*,*,#1679,.F.);
#2094=ORIENTED_EDGE('',*,*,#1685,.F.);
#2095=ORIENTED_EDGE('',*,*,#1681,.F.);
#2096=ORIENTED_EDGE('',*,*,#1686,.T.);
#2097=ORIENTED_EDGE('',*,*,#1687,.F.);
#2098=ORIENTED_EDGE('',*,*,#1680,.F.);
#2099=ORIENTED_EDGE('',*,*,#1684,.T.);
#2100=ORIENTED_EDGE('',*,*,#1688,.F.);
#2101=ORIENTED_EDGE('',*,*,#1686,.F.);
#2102=ORIENTED_EDGE('',*,*,#1689,.F.);
#2103=ORIENTED_EDGE('',*,*,#1687,.T.);
#2104=ORIENTED_EDGE('',*,*,#1688,.T.);
#2105=ORIENTED_EDGE('',*,*,#1683,.T.);
#2106=ORIENTED_EDGE('',*,*,#1665,.T.);
#2107=ORIENTED_EDGE('',*,*,#1690,.T.);
#2108=ORIENTED_EDGE('',*,*,#1691,.T.);
#2109=ORIENTED_EDGE('',*,*,#1692,.F.);
#2110=ORIENTED_EDGE('',*,*,#1693,.F.);
#2111=ORIENTED_EDGE('',*,*,#1694,.T.);
#2112=ORIENTED_EDGE('',*,*,#1693,.T.);
#2113=ORIENTED_EDGE('',*,*,#1695,.F.);
#2114=ORIENTED_EDGE('',*,*,#1696,.F.);
#2115=ORIENTED_EDGE('',*,*,#1697,.T.);
#2116=ORIENTED_EDGE('',*,*,#1696,.T.);
#2117=ORIENTED_EDGE('',*,*,#1698,.F.);
#2118=ORIENTED_EDGE('',*,*,#1699,.F.);
#2119=ORIENTED_EDGE('',*,*,#1700,.T.);
#2120=ORIENTED_EDGE('',*,*,#1699,.T.);
#2121=ORIENTED_EDGE('',*,*,#1701,.F.);
#2122=ORIENTED_EDGE('',*,*,#1691,.F.);
#2123=ORIENTED_EDGE('',*,*,#1701,.T.);
#2124=ORIENTED_EDGE('',*,*,#1698,.T.);
#2125=ORIENTED_EDGE('',*,*,#1695,.T.);
#2126=ORIENTED_EDGE('',*,*,#1692,.T.);
#2127=ORIENTED_EDGE('',*,*,#1630,.T.);
#2128=ORIENTED_EDGE('',*,*,#1639,.T.);
#2129=ORIENTED_EDGE('',*,*,#1634,.T.);
#2130=ORIENTED_EDGE('',*,*,#1641,.T.);
#2131=ORIENTED_EDGE('',*,*,#1644,.T.);
#2132=ORIENTED_EDGE('',*,*,#1647,.T.);
#2133=ORIENTED_EDGE('',*,*,#1655,.T.);
#2134=ORIENTED_EDGE('',*,*,#1651,.T.);
#2135=ORIENTED_EDGE('',*,*,#1658,.T.);
#2136=ORIENTED_EDGE('',*,*,#1662,.T.);
#2137=ORIENTED_EDGE('',*,*,#1670,.T.);
#2138=ORIENTED_EDGE('',*,*,#1666,.T.);
#2139=ORIENTED_EDGE('',*,*,#1673,.T.);
#2140=ORIENTED_EDGE('',*,*,#1677,.T.);
#2141=ORIENTED_EDGE('',*,*,#1682,.T.);
#2142=ORIENTED_EDGE('',*,*,#1678,.T.);
#2143=ORIENTED_EDGE('',*,*,#1685,.T.);
#2144=ORIENTED_EDGE('',*,*,#1689,.T.);
#2145=ORIENTED_EDGE('',*,*,#1700,.F.);
#2146=ORIENTED_EDGE('',*,*,#1690,.F.);
#2147=ORIENTED_EDGE('',*,*,#1694,.F.);
#2148=ORIENTED_EDGE('',*,*,#1697,.F.);
#2149=ORIENTED_EDGE('',*,*,#1642,.T.);
#2150=ORIENTED_EDGE('',*,*,#1645,.T.);
#2151=ORIENTED_EDGE('',*,*,#1702,.F.);
#2152=ORIENTED_EDGE('',*,*,#1702,.T.);
#2153=ORIENTED_EDGE('',*,*,#1703,.T.);
#2154=ORIENTED_EDGE('',*,*,#1704,.F.);
#2155=ORIENTED_EDGE('',*,*,#1703,.F.);
#2156=ORIENTED_EDGE('',*,*,#1705,.F.);
#2157=ORIENTED_EDGE('',*,*,#1706,.T.);
#2158=ORIENTED_EDGE('',*,*,#1707,.F.);
#2159=ORIENTED_EDGE('',*,*,#1708,.F.);
#2160=ORIENTED_EDGE('',*,*,#1709,.F.);
#2161=ORIENTED_EDGE('',*,*,#1710,.F.);
#2162=ORIENTED_EDGE('',*,*,#1711,.F.);
#2163=ORIENTED_EDGE('',*,*,#1712,.F.);
#2164=ORIENTED_EDGE('',*,*,#1706,.F.);
#2165=ORIENTED_EDGE('',*,*,#1711,.T.);
#2166=ORIENTED_EDGE('',*,*,#1713,.F.);
#2167=ORIENTED_EDGE('',*,*,#1714,.T.);
#2168=ORIENTED_EDGE('',*,*,#1715,.T.);
#2169=ORIENTED_EDGE('',*,*,#1710,.T.);
#2170=ORIENTED_EDGE('',*,*,#1716,.F.);
#2171=ORIENTED_EDGE('',*,*,#1717,.T.);
#2172=ORIENTED_EDGE('',*,*,#1713,.T.);
#2173=ORIENTED_EDGE('',*,*,#1709,.T.);
#2174=ORIENTED_EDGE('',*,*,#1718,.F.);
#2175=ORIENTED_EDGE('',*,*,#1719,.T.);
#2176=ORIENTED_EDGE('',*,*,#1716,.T.);
#2177=ORIENTED_EDGE('',*,*,#1708,.T.);
#2178=ORIENTED_EDGE('',*,*,#1720,.F.);
#2179=ORIENTED_EDGE('',*,*,#1721,.T.);
#2180=ORIENTED_EDGE('',*,*,#1718,.T.);
#2181=ORIENTED_EDGE('',*,*,#1707,.T.);
#2182=ORIENTED_EDGE('',*,*,#1722,.F.);
#2183=ORIENTED_EDGE('',*,*,#1723,.T.);
#2184=ORIENTED_EDGE('',*,*,#1720,.T.);
#2185=ORIENTED_EDGE('',*,*,#1712,.T.);
#2186=ORIENTED_EDGE('',*,*,#1715,.F.);
#2187=ORIENTED_EDGE('',*,*,#1724,.T.);
#2188=ORIENTED_EDGE('',*,*,#1722,.T.);
#2189=ORIENTED_EDGE('',*,*,#1705,.T.);
#2190=ORIENTED_EDGE('',*,*,#1719,.F.);
#2191=ORIENTED_EDGE('',*,*,#1721,.F.);
#2192=ORIENTED_EDGE('',*,*,#1723,.F.);
#2193=ORIENTED_EDGE('',*,*,#1724,.F.);
#2194=ORIENTED_EDGE('',*,*,#1714,.F.);
#2195=ORIENTED_EDGE('',*,*,#1717,.F.);
#2196=ORIENTED_EDGE('',*,*,#1704,.T.);
#2197=ORIENTED_EDGE('',*,*,#1725,.F.);
#2198=ORIENTED_EDGE('',*,*,#1726,.T.);
#2199=ORIENTED_EDGE('',*,*,#1727,.F.);
#2200=ORIENTED_EDGE('',*,*,#1726,.F.);
#2201=ORIENTED_EDGE('',*,*,#1728,.F.);
#2202=ORIENTED_EDGE('',*,*,#1729,.T.);
#2203=ORIENTED_EDGE('',*,*,#1730,.F.);
#2204=ORIENTED_EDGE('',*,*,#1729,.F.);
#2205=ORIENTED_EDGE('',*,*,#1731,.T.);
#2206=ORIENTED_EDGE('',*,*,#1732,.T.);
#2207=ORIENTED_EDGE('',*,*,#1733,.F.);
#2208=ORIENTED_EDGE('',*,*,#1734,.T.);
#2209=ORIENTED_EDGE('',*,*,#1735,.T.);
#2210=ORIENTED_EDGE('',*,*,#1736,.F.);
#2211=ORIENTED_EDGE('',*,*,#1731,.F.);
#2212=ORIENTED_EDGE('',*,*,#1737,.F.);
#2213=ORIENTED_EDGE('',*,*,#1738,.F.);
#2214=ORIENTED_EDGE('',*,*,#1739,.T.);
#2215=ORIENTED_EDGE('',*,*,#1740,.T.);
#2216=ORIENTED_EDGE('',*,*,#1741,.F.);
#2217=ORIENTED_EDGE('',*,*,#1742,.F.);
#2218=ORIENTED_EDGE('',*,*,#1743,.F.);
#2219=ORIENTED_EDGE('',*,*,#1744,.T.);
#2220=ORIENTED_EDGE('',*,*,#1739,.F.);
#2221=ORIENTED_EDGE('',*,*,#1745,.F.);
#2222=ORIENTED_EDGE('',*,*,#1746,.T.);
#2223=ORIENTED_EDGE('',*,*,#1747,.T.);
#2224=ORIENTED_EDGE('',*,*,#1748,.F.);
#2225=ORIENTED_EDGE('',*,*,#1749,.T.);
#2226=ORIENTED_EDGE('',*,*,#1745,.T.);
#2227=ORIENTED_EDGE('',*,*,#1738,.T.);
#2228=ORIENTED_EDGE('',*,*,#1737,.T.);
#2229=ORIENTED_EDGE('',*,*,#1735,.F.);
#2230=ORIENTED_EDGE('',*,*,#1750,.T.);
#2231=ORIENTED_EDGE('',*,*,#1746,.F.);
#2232=ORIENTED_EDGE('',*,*,#1751,.F.);
#2233=ORIENTED_EDGE('',*,*,#1747,.F.);
#2234=ORIENTED_EDGE('',*,*,#1750,.F.);
#2235=ORIENTED_EDGE('',*,*,#1734,.F.);
#2236=ORIENTED_EDGE('',*,*,#1736,.T.);
#2237=ORIENTED_EDGE('',*,*,#1749,.F.);
#2238=ORIENTED_EDGE('',*,*,#1752,.F.);
#2239=ORIENTED_EDGE('',*,*,#1732,.F.);
#2240=ORIENTED_EDGE('',*,*,#1742,.T.);
#2241=ORIENTED_EDGE('',*,*,#1753,.T.);
#2242=ORIENTED_EDGE('',*,*,#1754,.T.);
#2243=ORIENTED_EDGE('',*,*,#1755,.F.);
#2244=ORIENTED_EDGE('',*,*,#1756,.T.);
#2245=ORIENTED_EDGE('',*,*,#1741,.T.);
#2246=ORIENTED_EDGE('',*,*,#1757,.F.);
#2247=ORIENTED_EDGE('',*,*,#1758,.T.);
#2248=ORIENTED_EDGE('',*,*,#1753,.F.);
#2249=ORIENTED_EDGE('',*,*,#1759,.T.);
#2250=ORIENTED_EDGE('',*,*,#1760,.F.);
#2251=ORIENTED_EDGE('',*,*,#1761,.T.);
#2252=ORIENTED_EDGE('',*,*,#1757,.T.);
#2253=ORIENTED_EDGE('',*,*,#1740,.F.);
#2254=ORIENTED_EDGE('',*,*,#1744,.F.);
#2255=ORIENTED_EDGE('',*,*,#1762,.F.);
#2256=ORIENTED_EDGE('',*,*,#1754,.F.);
#2257=ORIENTED_EDGE('',*,*,#1758,.F.);
#2258=ORIENTED_EDGE('',*,*,#1761,.F.);
#2259=ORIENTED_EDGE('',*,*,#1743,.T.);
#2260=ORIENTED_EDGE('',*,*,#1756,.F.);
#2261=ORIENTED_EDGE('',*,*,#1763,.F.);
#2262=ORIENTED_EDGE('',*,*,#1759,.F.);
#2263=ORIENTED_EDGE('',*,*,#1764,.T.);
#2264=ORIENTED_EDGE('',*,*,#1765,.T.);
#2265=ORIENTED_EDGE('',*,*,#1766,.F.);
#2266=ORIENTED_EDGE('',*,*,#1767,.F.);
#2267=ORIENTED_EDGE('',*,*,#1768,.T.);
#2268=ORIENTED_EDGE('',*,*,#1767,.T.);
#2269=ORIENTED_EDGE('',*,*,#1769,.F.);
#2270=ORIENTED_EDGE('',*,*,#1770,.F.);
#2271=ORIENTED_EDGE('',*,*,#1771,.T.);
#2272=ORIENTED_EDGE('',*,*,#1770,.T.);
#2273=ORIENTED_EDGE('',*,*,#1772,.F.);
#2274=ORIENTED_EDGE('',*,*,#1773,.F.);
#2275=ORIENTED_EDGE('',*,*,#1774,.T.);
#2276=ORIENTED_EDGE('',*,*,#1773,.T.);
#2277=ORIENTED_EDGE('',*,*,#1775,.F.);
#2278=ORIENTED_EDGE('',*,*,#1765,.F.);
#2279=ORIENTED_EDGE('',*,*,#1775,.T.);
#2280=ORIENTED_EDGE('',*,*,#1772,.T.);
#2281=ORIENTED_EDGE('',*,*,#1769,.T.);
#2282=ORIENTED_EDGE('',*,*,#1766,.T.);
#2283=ORIENTED_EDGE('',*,*,#1727,.T.);
#2284=ORIENTED_EDGE('',*,*,#1730,.T.);
#2285=ORIENTED_EDGE('',*,*,#1751,.T.);
#2286=ORIENTED_EDGE('',*,*,#1733,.T.);
#2287=ORIENTED_EDGE('',*,*,#1752,.T.);
#2288=ORIENTED_EDGE('',*,*,#1748,.T.);
#2289=ORIENTED_EDGE('',*,*,#1762,.T.);
#2290=ORIENTED_EDGE('',*,*,#1760,.T.);
#2291=ORIENTED_EDGE('',*,*,#1763,.T.);
#2292=ORIENTED_EDGE('',*,*,#1755,.T.);
#2293=ORIENTED_EDGE('',*,*,#1774,.F.);
#2294=ORIENTED_EDGE('',*,*,#1764,.F.);
#2295=ORIENTED_EDGE('',*,*,#1768,.F.);
#2296=ORIENTED_EDGE('',*,*,#1771,.F.);
#2297=ORIENTED_EDGE('',*,*,#1725,.T.);
#2298=ORIENTED_EDGE('',*,*,#1728,.T.);
#2299=ORIENTED_EDGE('',*,*,#1776,.F.);
#2300=ORIENTED_EDGE('',*,*,#1777,.T.);
#2301=ORIENTED_EDGE('',*,*,#1778,.F.);
#2302=ORIENTED_EDGE('',*,*,#1777,.F.);
#2303=ORIENTED_EDGE('',*,*,#1779,.F.);
#2304=ORIENTED_EDGE('',*,*,#1780,.T.);
#2305=ORIENTED_EDGE('',*,*,#1781,.F.);
#2306=ORIENTED_EDGE('',*,*,#1780,.F.);
#2307=ORIENTED_EDGE('',*,*,#1782,.F.);
#2308=ORIENTED_EDGE('',*,*,#1783,.T.);
#2309=ORIENTED_EDGE('',*,*,#1784,.F.);
#2310=ORIENTED_EDGE('',*,*,#1783,.F.);
#2311=ORIENTED_EDGE('',*,*,#1785,.F.);
#2312=ORIENTED_EDGE('',*,*,#1786,.F.);
#2313=ORIENTED_EDGE('',*,*,#1787,.F.);
#2314=ORIENTED_EDGE('',*,*,#1788,.T.);
#2315=ORIENTED_EDGE('',*,*,#1788,.F.);
#2316=ORIENTED_EDGE('',*,*,#1789,.F.);
#2317=ORIENTED_EDGE('',*,*,#1790,.F.);
#2318=ORIENTED_EDGE('',*,*,#1791,.F.);
#2319=ORIENTED_EDGE('',*,*,#1792,.F.);
#2320=ORIENTED_EDGE('',*,*,#1793,.F.);
#2321=ORIENTED_EDGE('',*,*,#1794,.F.);
#2322=ORIENTED_EDGE('',*,*,#1795,.F.);
#2323=ORIENTED_EDGE('',*,*,#1776,.T.);
#2324=ORIENTED_EDGE('',*,*,#1779,.T.);
#2325=ORIENTED_EDGE('',*,*,#1782,.T.);
#2326=ORIENTED_EDGE('',*,*,#1787,.T.);
#2327=ORIENTED_EDGE('',*,*,#1796,.F.);
#2328=ORIENTED_EDGE('',*,*,#1797,.T.);
#2329=ORIENTED_EDGE('',*,*,#1789,.T.);
#2330=ORIENTED_EDGE('',*,*,#1797,.F.);
#2331=ORIENTED_EDGE('',*,*,#1798,.F.);
#2332=ORIENTED_EDGE('',*,*,#1799,.F.);
#2333=ORIENTED_EDGE('',*,*,#1790,.T.);
#2334=ORIENTED_EDGE('',*,*,#1800,.F.);
#2335=ORIENTED_EDGE('',*,*,#1794,.T.);
#2336=ORIENTED_EDGE('',*,*,#1801,.F.);
#2337=ORIENTED_EDGE('',*,*,#1802,.F.);
#2338=ORIENTED_EDGE('',*,*,#1803,.T.);
#2339=ORIENTED_EDGE('',*,*,#1802,.T.);
#2340=ORIENTED_EDGE('',*,*,#1804,.T.);
#2341=ORIENTED_EDGE('',*,*,#1805,.T.);
#2342=ORIENTED_EDGE('',*,*,#1806,.T.);
#2343=ORIENTED_EDGE('',*,*,#1798,.T.);
#2344=ORIENTED_EDGE('',*,*,#1796,.T.);
#2345=ORIENTED_EDGE('',*,*,#1786,.T.);
#2346=ORIENTED_EDGE('',*,*,#1778,.T.);
#2347=ORIENTED_EDGE('',*,*,#1781,.T.);
#2348=ORIENTED_EDGE('',*,*,#1784,.T.);
#2349=ORIENTED_EDGE('',*,*,#1801,.T.);
#2350=ORIENTED_EDGE('',*,*,#1793,.T.);
#2351=ORIENTED_EDGE('',*,*,#1807,.F.);
#2352=ORIENTED_EDGE('',*,*,#1804,.F.);
#2353=ORIENTED_EDGE('',*,*,#1799,.T.);
#2354=ORIENTED_EDGE('',*,*,#1806,.F.);
#2355=ORIENTED_EDGE('',*,*,#1808,.F.);
#2356=ORIENTED_EDGE('',*,*,#1791,.T.);
#2357=ORIENTED_EDGE('',*,*,#1785,.T.);
#2358=ORIENTED_EDGE('',*,*,#1795,.T.);
#2359=ORIENTED_EDGE('',*,*,#1800,.T.);
#2360=ORIENTED_EDGE('',*,*,#1803,.F.);
#2361=ORIENTED_EDGE('',*,*,#1807,.T.);
#2362=ORIENTED_EDGE('',*,*,#1792,.T.);
#2363=ORIENTED_EDGE('',*,*,#1808,.T.);
#2364=ORIENTED_EDGE('',*,*,#1805,.F.);
#2365=ORIENTED_EDGE('',*,*,#1809,.F.);
#2366=ORIENTED_EDGE('',*,*,#1810,.T.);
#2367=ORIENTED_EDGE('',*,*,#1811,.T.);
#2368=ORIENTED_EDGE('',*,*,#1810,.F.);
#2369=ORIENTED_EDGE('',*,*,#1812,.F.);
#2370=ORIENTED_EDGE('',*,*,#1813,.T.);
#2371=ORIENTED_EDGE('',*,*,#1814,.T.);
#2372=ORIENTED_EDGE('',*,*,#1813,.F.);
#2373=ORIENTED_EDGE('',*,*,#1812,.T.);
#2374=ORIENTED_EDGE('',*,*,#1809,.T.);
#2375=ORIENTED_EDGE('',*,*,#1814,.F.);
#2376=ORIENTED_EDGE('',*,*,#1811,.F.);
#2377=ORIENTED_EDGE('',*,*,#1815,.F.);
#2378=ORIENTED_EDGE('',*,*,#1816,.T.);
#2379=ORIENTED_EDGE('',*,*,#1817,.T.);
#2380=ORIENTED_EDGE('',*,*,#1816,.F.);
#2381=ORIENTED_EDGE('',*,*,#1818,.F.);
#2382=ORIENTED_EDGE('',*,*,#1819,.T.);
#2383=ORIENTED_EDGE('',*,*,#1820,.T.);
#2384=ORIENTED_EDGE('',*,*,#1819,.F.);
#2385=ORIENTED_EDGE('',*,*,#1818,.T.);
#2386=ORIENTED_EDGE('',*,*,#1815,.T.);
#2387=ORIENTED_EDGE('',*,*,#1820,.F.);
#2388=ORIENTED_EDGE('',*,*,#1817,.F.);
#2389=ORIENTED_EDGE('',*,*,#1821,.F.);
#2390=ORIENTED_EDGE('',*,*,#1822,.T.);
#2391=ORIENTED_EDGE('',*,*,#1823,.F.);
#2392=ORIENTED_EDGE('',*,*,#1822,.F.);
#2393=ORIENTED_EDGE('',*,*,#1821,.T.);
#2394=ORIENTED_EDGE('',*,*,#1824,.F.);
#2395=ORIENTED_EDGE('',*,*,#1825,.T.);
#2396=ORIENTED_EDGE('',*,*,#1826,.T.);
#2397=ORIENTED_EDGE('',*,*,#1825,.F.);
#2398=ORIENTED_EDGE('',*,*,#1824,.T.);
#2399=ORIENTED_EDGE('',*,*,#1823,.T.);
#2400=ORIENTED_EDGE('',*,*,#1826,.F.);
#2401=ORIENTED_EDGE('',*,*,#1827,.T.);
#2402=ORIENTED_EDGE('',*,*,#1828,.T.);
#2403=ORIENTED_EDGE('',*,*,#1829,.T.);
#2404=ORIENTED_EDGE('',*,*,#1830,.F.);
#2405=ORIENTED_EDGE('',*,*,#1831,.T.);
#2406=ORIENTED_EDGE('',*,*,#1832,.T.);
#2407=ORIENTED_EDGE('',*,*,#1833,.T.);
#2408=ORIENTED_EDGE('',*,*,#1828,.F.);
#2409=ORIENTED_EDGE('',*,*,#1834,.T.);
#2410=ORIENTED_EDGE('',*,*,#1835,.T.);
#2411=ORIENTED_EDGE('',*,*,#1836,.T.);
#2412=ORIENTED_EDGE('',*,*,#1832,.F.);
#2413=ORIENTED_EDGE('',*,*,#1837,.T.);
#2414=ORIENTED_EDGE('',*,*,#1838,.T.);
#2415=ORIENTED_EDGE('',*,*,#1839,.T.);
#2416=ORIENTED_EDGE('',*,*,#1835,.F.);
#2417=ORIENTED_EDGE('',*,*,#1840,.T.);
#2418=ORIENTED_EDGE('',*,*,#1841,.T.);
#2419=ORIENTED_EDGE('',*,*,#1842,.T.);
#2420=ORIENTED_EDGE('',*,*,#1838,.F.);
#2421=ORIENTED_EDGE('',*,*,#1843,.T.);
#2422=ORIENTED_EDGE('',*,*,#1830,.T.);
#2423=ORIENTED_EDGE('',*,*,#1844,.T.);
#2424=ORIENTED_EDGE('',*,*,#1841,.F.);
#2425=ORIENTED_EDGE('',*,*,#1843,.F.);
#2426=ORIENTED_EDGE('',*,*,#1840,.F.);
#2427=ORIENTED_EDGE('',*,*,#1837,.F.);
#2428=ORIENTED_EDGE('',*,*,#1834,.F.);
#2429=ORIENTED_EDGE('',*,*,#1831,.F.);
#2430=ORIENTED_EDGE('',*,*,#1827,.F.);
#2431=ORIENTED_EDGE('',*,*,#1844,.F.);
#2432=ORIENTED_EDGE('',*,*,#1829,.F.);
#2433=ORIENTED_EDGE('',*,*,#1833,.F.);
#2434=ORIENTED_EDGE('',*,*,#1836,.F.);
#2435=ORIENTED_EDGE('',*,*,#1839,.F.);
#2436=ORIENTED_EDGE('',*,*,#1842,.F.);
#2437=ORIENTED_EDGE('',*,*,#1845,.F.);
#2438=ORIENTED_EDGE('',*,*,#1846,.F.);
#2439=ORIENTED_EDGE('',*,*,#1847,.F.);
#2440=ORIENTED_EDGE('',*,*,#1848,.T.);
#2441=ORIENTED_EDGE('',*,*,#1846,.T.);
#2442=ORIENTED_EDGE('',*,*,#1848,.F.);
#2443=ORIENTED_EDGE('',*,*,#1849,.F.);
#2444=ORIENTED_EDGE('',*,*,#1850,.T.);
#2445=ORIENTED_EDGE('',*,*,#1847,.T.);
#2446=ORIENTED_EDGE('',*,*,#1850,.F.);
#2447=ORIENTED_EDGE('',*,*,#1851,.F.);
#2448=ORIENTED_EDGE('',*,*,#1852,.T.);
#2449=ORIENTED_EDGE('',*,*,#1849,.T.);
#2450=ORIENTED_EDGE('',*,*,#1852,.F.);
#2451=ORIENTED_EDGE('',*,*,#1851,.T.);
#2452=ORIENTED_EDGE('',*,*,#1853,.F.);
#2453=ORIENTED_EDGE('',*,*,#1854,.F.);
#2454=ORIENTED_EDGE('',*,*,#1855,.T.);
#2455=ORIENTED_EDGE('',*,*,#1853,.T.);
#2456=ORIENTED_EDGE('',*,*,#1855,.F.);
#2457=ORIENTED_EDGE('',*,*,#1845,.T.);
#2458=ORIENTED_EDGE('',*,*,#1856,.T.);
#2459=ORIENTED_EDGE('',*,*,#1854,.T.);
#2460=ORIENTED_EDGE('',*,*,#1856,.F.);
#2461=ORIENTED_EDGE('',*,*,#1857,.F.);
#2462=ORIENTED_EDGE('',*,*,#1858,.T.);
#2463=ORIENTED_EDGE('',*,*,#1859,.F.);
#2464=ORIENTED_EDGE('',*,*,#1858,.F.);
#2465=ORIENTED_EDGE('',*,*,#1860,.F.);
#2466=ORIENTED_EDGE('',*,*,#1861,.T.);
#2467=ORIENTED_EDGE('',*,*,#1862,.F.);
#2468=ORIENTED_EDGE('',*,*,#1861,.F.);
#2469=ORIENTED_EDGE('',*,*,#1863,.F.);
#2470=ORIENTED_EDGE('',*,*,#1864,.F.);
#2471=ORIENTED_EDGE('',*,*,#1865,.F.);
#2472=ORIENTED_EDGE('',*,*,#1866,.T.);
#2473=ORIENTED_EDGE('',*,*,#1863,.T.);
#2474=ORIENTED_EDGE('',*,*,#1867,.T.);
#2475=ORIENTED_EDGE('',*,*,#1868,.F.);
#2476=ORIENTED_EDGE('',*,*,#1869,.F.);
#2477=ORIENTED_EDGE('',*,*,#1866,.F.);
#2478=ORIENTED_EDGE('',*,*,#1870,.F.);
#2479=ORIENTED_EDGE('',*,*,#1871,.F.);
#2480=ORIENTED_EDGE('',*,*,#1867,.F.);
#2481=ORIENTED_EDGE('',*,*,#1857,.T.);
#2482=ORIENTED_EDGE('',*,*,#1860,.T.);
#2483=ORIENTED_EDGE('',*,*,#1865,.T.);
#2484=ORIENTED_EDGE('',*,*,#1872,.F.);
#2485=ORIENTED_EDGE('',*,*,#1873,.F.);
#2486=ORIENTED_EDGE('',*,*,#1870,.T.);
#2487=ORIENTED_EDGE('',*,*,#1868,.T.);
#2488=ORIENTED_EDGE('',*,*,#1871,.T.);
#2489=ORIENTED_EDGE('',*,*,#1873,.T.);
#2490=ORIENTED_EDGE('',*,*,#1874,.F.);
#2491=ORIENTED_EDGE('',*,*,#1869,.T.);
#2492=ORIENTED_EDGE('',*,*,#1874,.T.);
#2493=ORIENTED_EDGE('',*,*,#1872,.T.);
#2494=ORIENTED_EDGE('',*,*,#1864,.T.);
#2495=ORIENTED_EDGE('',*,*,#1859,.T.);
#2496=ORIENTED_EDGE('',*,*,#1862,.T.);
#2497=ORIENTED_EDGE('',*,*,#1875,.F.);
#2498=ORIENTED_EDGE('',*,*,#1876,.T.);
#2499=ORIENTED_EDGE('',*,*,#1877,.F.);
#2500=ORIENTED_EDGE('',*,*,#1876,.F.);
#2501=ORIENTED_EDGE('',*,*,#1875,.T.);
#2502=ORIENTED_EDGE('',*,*,#1878,.F.);
#2503=ORIENTED_EDGE('',*,*,#1879,.T.);
#2504=ORIENTED_EDGE('',*,*,#1880,.F.);
#2505=ORIENTED_EDGE('',*,*,#1879,.F.);
#2506=ORIENTED_EDGE('',*,*,#1881,.F.);
#2507=ORIENTED_EDGE('',*,*,#1882,.T.);
#2508=ORIENTED_EDGE('',*,*,#1883,.F.);
#2509=ORIENTED_EDGE('',*,*,#1882,.F.);
#2510=ORIENTED_EDGE('',*,*,#1884,.F.);
#2511=ORIENTED_EDGE('',*,*,#1885,.F.);
#2512=ORIENTED_EDGE('',*,*,#1886,.F.);
#2513=ORIENTED_EDGE('',*,*,#1887,.F.);
#2514=ORIENTED_EDGE('',*,*,#1878,.T.);
#2515=ORIENTED_EDGE('',*,*,#1881,.T.);
#2516=ORIENTED_EDGE('',*,*,#1888,.T.);
#2517=ORIENTED_EDGE('',*,*,#1885,.T.);
#2518=ORIENTED_EDGE('',*,*,#1889,.T.);
#2519=ORIENTED_EDGE('',*,*,#1890,.F.);
#2520=ORIENTED_EDGE('',*,*,#1891,.F.);
#2521=ORIENTED_EDGE('',*,*,#1886,.T.);
#2522=ORIENTED_EDGE('',*,*,#1891,.T.);
#2523=ORIENTED_EDGE('',*,*,#1892,.F.);
#2524=ORIENTED_EDGE('',*,*,#1893,.F.);
#2525=ORIENTED_EDGE('',*,*,#1887,.T.);
#2526=ORIENTED_EDGE('',*,*,#1893,.T.);
#2527=ORIENTED_EDGE('',*,*,#1894,.F.);
#2528=ORIENTED_EDGE('',*,*,#1895,.F.);
#2529=ORIENTED_EDGE('',*,*,#1884,.T.);
#2530=ORIENTED_EDGE('',*,*,#1895,.T.);
#2531=ORIENTED_EDGE('',*,*,#1896,.F.);
#2532=ORIENTED_EDGE('',*,*,#1889,.F.);
#2533=ORIENTED_EDGE('',*,*,#1896,.T.);
#2534=ORIENTED_EDGE('',*,*,#1894,.T.);
#2535=ORIENTED_EDGE('',*,*,#1892,.T.);
#2536=ORIENTED_EDGE('',*,*,#1890,.T.);
#2537=ORIENTED_EDGE('',*,*,#1877,.T.);
#2538=ORIENTED_EDGE('',*,*,#1880,.T.);
#2539=ORIENTED_EDGE('',*,*,#1883,.T.);
#2540=ORIENTED_EDGE('',*,*,#1897,.F.);
#2541=ORIENTED_EDGE('',*,*,#1898,.T.);
#2542=ORIENTED_EDGE('',*,*,#1899,.F.);
#2543=ORIENTED_EDGE('',*,*,#1898,.F.);
#2544=ORIENTED_EDGE('',*,*,#1900,.T.);
#2545=ORIENTED_EDGE('',*,*,#1901,.F.);
#2546=ORIENTED_EDGE('',*,*,#1902,.F.);
#2547=ORIENTED_EDGE('',*,*,#1903,.T.);
#2548=ORIENTED_EDGE('',*,*,#1904,.T.);
#2549=ORIENTED_EDGE('',*,*,#1905,.T.);
#2550=ORIENTED_EDGE('',*,*,#1906,.T.);
#2551=ORIENTED_EDGE('',*,*,#1903,.F.);
#2552=ORIENTED_EDGE('',*,*,#1897,.T.);
#2553=ORIENTED_EDGE('',*,*,#1905,.F.);
#2554=ORIENTED_EDGE('',*,*,#1907,.F.);
#2555=ORIENTED_EDGE('',*,*,#1908,.F.);
#2556=ORIENTED_EDGE('',*,*,#1909,.T.);
#2557=ORIENTED_EDGE('',*,*,#1910,.T.);
#2558=ORIENTED_EDGE('',*,*,#1908,.T.);
#2559=ORIENTED_EDGE('',*,*,#1911,.T.);
#2560=ORIENTED_EDGE('',*,*,#1912,.F.);
#2561=ORIENTED_EDGE('',*,*,#1904,.F.);
#2562=ORIENTED_EDGE('',*,*,#1902,.T.);
#2563=ORIENTED_EDGE('',*,*,#1913,.F.);
#2564=ORIENTED_EDGE('',*,*,#1914,.F.);
#2565=ORIENTED_EDGE('',*,*,#1911,.F.);
#2566=ORIENTED_EDGE('',*,*,#1907,.T.);
#2567=ORIENTED_EDGE('',*,*,#1915,.F.);
#2568=ORIENTED_EDGE('',*,*,#1900,.F.);
#2569=ORIENTED_EDGE('',*,*,#1906,.F.);
#2570=ORIENTED_EDGE('',*,*,#1909,.F.);
#2571=ORIENTED_EDGE('',*,*,#1910,.F.);
#2572=ORIENTED_EDGE('',*,*,#1916,.T.);
#2573=ORIENTED_EDGE('',*,*,#1914,.T.);
#2574=ORIENTED_EDGE('',*,*,#1917,.F.);
#2575=ORIENTED_EDGE('',*,*,#1916,.F.);
#2576=ORIENTED_EDGE('',*,*,#1918,.F.);
#2577=ORIENTED_EDGE('',*,*,#1915,.T.);
#2578=ORIENTED_EDGE('',*,*,#1917,.T.);
#2579=ORIENTED_EDGE('',*,*,#1913,.T.);
#2580=ORIENTED_EDGE('',*,*,#1901,.T.);
#2581=ORIENTED_EDGE('',*,*,#1899,.T.);
#2582=ORIENTED_EDGE('',*,*,#1912,.T.);
#2583=ORIENTED_EDGE('',*,*,#1919,.F.);
#2584=ORIENTED_EDGE('',*,*,#1888,.F.);
#2585=ORIENTED_EDGE('',*,*,#1920,.T.);
#2586=ORIENTED_EDGE('',*,*,#1919,.T.);
#2587=ORIENTED_EDGE('',*,*,#1918,.T.);
#2588=ORIENTED_EDGE('',*,*,#1920,.F.);
#2589=ORIENTED_EDGE('',*,*,#1921,.F.);
#2590=ORIENTED_EDGE('',*,*,#1922,.T.);
#2591=ORIENTED_EDGE('',*,*,#1923,.T.);
#2592=ORIENTED_EDGE('',*,*,#1922,.F.);
#2593=ORIENTED_EDGE('',*,*,#1924,.F.);
#2594=ORIENTED_EDGE('',*,*,#1925,.T.);
#2595=ORIENTED_EDGE('',*,*,#1926,.T.);
#2596=ORIENTED_EDGE('',*,*,#1925,.F.);
#2597=ORIENTED_EDGE('',*,*,#1924,.T.);
#2598=ORIENTED_EDGE('',*,*,#1921,.T.);
#2599=ORIENTED_EDGE('',*,*,#1926,.F.);
#2600=ORIENTED_EDGE('',*,*,#1923,.F.);
#2601=ORIENTED_EDGE('',*,*,#1927,.F.);
#2602=ORIENTED_EDGE('',*,*,#1928,.T.);
#2603=ORIENTED_EDGE('',*,*,#1929,.F.);
#2604=ORIENTED_EDGE('',*,*,#1928,.F.);
#2605=ORIENTED_EDGE('',*,*,#1930,.F.);
#2606=ORIENTED_EDGE('',*,*,#1931,.F.);
#2607=ORIENTED_EDGE('',*,*,#1932,.F.);
#2608=ORIENTED_EDGE('',*,*,#1933,.F.);
#2609=ORIENTED_EDGE('',*,*,#1934,.T.);
#2610=ORIENTED_EDGE('',*,*,#1932,.T.);
#2611=ORIENTED_EDGE('',*,*,#1934,.F.);
#2612=ORIENTED_EDGE('',*,*,#1935,.F.);
#2613=ORIENTED_EDGE('',*,*,#1936,.T.);
#2614=ORIENTED_EDGE('',*,*,#1933,.T.);
#2615=ORIENTED_EDGE('',*,*,#1936,.F.);
#2616=ORIENTED_EDGE('',*,*,#1935,.T.);
#2617=ORIENTED_EDGE('',*,*,#1937,.F.);
#2618=ORIENTED_EDGE('',*,*,#1938,.F.);
#2619=ORIENTED_EDGE('',*,*,#1939,.T.);
#2620=ORIENTED_EDGE('',*,*,#1931,.T.);
#2621=ORIENTED_EDGE('',*,*,#1940,.T.);
#2622=ORIENTED_EDGE('',*,*,#1937,.T.);
#2623=ORIENTED_EDGE('',*,*,#1940,.F.);
#2624=ORIENTED_EDGE('',*,*,#1930,.T.);
#2625=ORIENTED_EDGE('',*,*,#1927,.T.);
#2626=ORIENTED_EDGE('',*,*,#1939,.F.);
#2627=ORIENTED_EDGE('',*,*,#1929,.T.);
#2628=ORIENTED_EDGE('',*,*,#1941,.F.);
#2629=ORIENTED_EDGE('',*,*,#1942,.T.);
#2630=ORIENTED_EDGE('',*,*,#1938,.T.);
#2631=ORIENTED_EDGE('',*,*,#1942,.F.);
#2632=ORIENTED_EDGE('',*,*,#1941,.T.);
#2633=ORIENTED_EDGE('',*,*,#1943,.F.);
#2634=ORIENTED_EDGE('',*,*,#1944,.T.);
#2635=ORIENTED_EDGE('',*,*,#1945,.T.);
#2636=ORIENTED_EDGE('',*,*,#1944,.F.);
#2637=ORIENTED_EDGE('',*,*,#1946,.F.);
#2638=ORIENTED_EDGE('',*,*,#1947,.T.);
#2639=ORIENTED_EDGE('',*,*,#1948,.T.);
#2640=ORIENTED_EDGE('',*,*,#1947,.F.);
#2641=ORIENTED_EDGE('',*,*,#1946,.T.);
#2642=ORIENTED_EDGE('',*,*,#1943,.T.);
#2643=ORIENTED_EDGE('',*,*,#1948,.F.);
#2644=ORIENTED_EDGE('',*,*,#1945,.F.);
#2645=ORIENTED_EDGE('',*,*,#1949,.F.);
#2646=ORIENTED_EDGE('',*,*,#1950,.T.);
#2647=ORIENTED_EDGE('',*,*,#1949,.T.);
#2648=ORIENTED_EDGE('',*,*,#1950,.F.);
#2649=ORIENTED_EDGE('',*,*,#1951,.F.);
#2650=ORIENTED_EDGE('',*,*,#1952,.F.);
#2651=ORIENTED_EDGE('',*,*,#1953,.T.);
#2652=ORIENTED_EDGE('',*,*,#1954,.F.);
#2653=ORIENTED_EDGE('',*,*,#1954,.T.);
#2654=ORIENTED_EDGE('',*,*,#1955,.T.);
#2655=ORIENTED_EDGE('',*,*,#1956,.F.);
#2656=ORIENTED_EDGE('',*,*,#1957,.F.);
#2657=ORIENTED_EDGE('',*,*,#1953,.F.);
#2658=ORIENTED_EDGE('',*,*,#1957,.T.);
#2659=ORIENTED_EDGE('',*,*,#1958,.F.);
#2660=ORIENTED_EDGE('',*,*,#1959,.T.);
#2661=ORIENTED_EDGE('',*,*,#1952,.T.);
#2662=ORIENTED_EDGE('',*,*,#1951,.T.);
#2663=ORIENTED_EDGE('',*,*,#1959,.F.);
#2664=ORIENTED_EDGE('',*,*,#1960,.F.);
#2665=ORIENTED_EDGE('',*,*,#1955,.F.);
#2666=ORIENTED_EDGE('',*,*,#1960,.T.);
#2667=ORIENTED_EDGE('',*,*,#1958,.T.);
#2668=ORIENTED_EDGE('',*,*,#1956,.T.);
#2669=ORIENTED_EDGE('',*,*,#1961,.F.);
#2670=ORIENTED_EDGE('',*,*,#1962,.T.);
#2671=ORIENTED_EDGE('',*,*,#1963,.T.);
#2672=ORIENTED_EDGE('',*,*,#1964,.T.);
#2673=ORIENTED_EDGE('',*,*,#1962,.F.);
#2674=ORIENTED_EDGE('',*,*,#1963,.F.);
#2675=ORIENTED_EDGE('',*,*,#1964,.F.);
#2676=ORIENTED_EDGE('',*,*,#1965,.T.);
#2677=ORIENTED_EDGE('',*,*,#1966,.T.);
#2678=ORIENTED_EDGE('',*,*,#1967,.T.);
#2679=ORIENTED_EDGE('',*,*,#1965,.F.);
#2680=ORIENTED_EDGE('',*,*,#1967,.F.);
#2681=ORIENTED_EDGE('',*,*,#1968,.T.);
#2682=ORIENTED_EDGE('',*,*,#1969,.T.);
#2683=ORIENTED_EDGE('',*,*,#1968,.F.);
#2684=ORIENTED_EDGE('',*,*,#1966,.F.);
#2685=ORIENTED_EDGE('',*,*,#1961,.T.);
#2686=ORIENTED_EDGE('',*,*,#1969,.F.);
#2687=ORIENTED_EDGE('',*,*,#1970,.F.);
#2688=ORIENTED_EDGE('',*,*,#1971,.T.);
#2689=ORIENTED_EDGE('',*,*,#1972,.T.);
#2690=ORIENTED_EDGE('',*,*,#1971,.F.);
#2691=ORIENTED_EDGE('',*,*,#1973,.F.);
#2692=ORIENTED_EDGE('',*,*,#1974,.T.);
#2693=ORIENTED_EDGE('',*,*,#1975,.T.);
#2694=ORIENTED_EDGE('',*,*,#1974,.F.);
#2695=ORIENTED_EDGE('',*,*,#1973,.T.);
#2696=ORIENTED_EDGE('',*,*,#1970,.T.);
#2697=ORIENTED_EDGE('',*,*,#1975,.F.);
#2698=ORIENTED_EDGE('',*,*,#1972,.F.);
#2699=ORIENTED_EDGE('',*,*,#1976,.F.);
#2700=ORIENTED_EDGE('',*,*,#1977,.F.);
#2701=ORIENTED_EDGE('',*,*,#1978,.T.);
#2702=ORIENTED_EDGE('',*,*,#1979,.F.);
#2703=ORIENTED_EDGE('',*,*,#1978,.F.);
#2704=ORIENTED_EDGE('',*,*,#1980,.F.);
#2705=ORIENTED_EDGE('',*,*,#1981,.F.);
#2706=ORIENTED_EDGE('',*,*,#1982,.F.);
#2707=ORIENTED_EDGE('',*,*,#1983,.F.);
#2708=ORIENTED_EDGE('',*,*,#1984,.F.);
#2709=ORIENTED_EDGE('',*,*,#1985,.T.);
#2710=ORIENTED_EDGE('',*,*,#1986,.F.);
#2711=ORIENTED_EDGE('',*,*,#1987,.F.);
#2712=ORIENTED_EDGE('',*,*,#1988,.F.);
#2713=ORIENTED_EDGE('',*,*,#1989,.F.);
#2714=ORIENTED_EDGE('',*,*,#1990,.F.);
#2715=ORIENTED_EDGE('',*,*,#1991,.F.);
#2716=ORIENTED_EDGE('',*,*,#1985,.F.);
#2717=ORIENTED_EDGE('',*,*,#1981,.T.);
#2718=ORIENTED_EDGE('',*,*,#1992,.T.);
#2719=ORIENTED_EDGE('',*,*,#1990,.T.);
#2720=ORIENTED_EDGE('',*,*,#1993,.F.);
#2721=ORIENTED_EDGE('',*,*,#1980,.T.);
#2722=ORIENTED_EDGE('',*,*,#1994,.T.);
#2723=ORIENTED_EDGE('',*,*,#1991,.T.);
#2724=ORIENTED_EDGE('',*,*,#1992,.F.);
#2725=ORIENTED_EDGE('',*,*,#1977,.T.);
#2726=ORIENTED_EDGE('',*,*,#1995,.T.);
#2727=ORIENTED_EDGE('',*,*,#1986,.T.);
#2728=ORIENTED_EDGE('',*,*,#1994,.F.);
#2729=ORIENTED_EDGE('',*,*,#1996,.F.);
#2730=ORIENTED_EDGE('',*,*,#1997,.T.);
#2731=ORIENTED_EDGE('',*,*,#1998,.T.);
#2732=ORIENTED_EDGE('',*,*,#1997,.F.);
#2733=ORIENTED_EDGE('',*,*,#1976,.T.);
#2734=ORIENTED_EDGE('',*,*,#1999,.T.);
#2735=ORIENTED_EDGE('',*,*,#1987,.T.);
#2736=ORIENTED_EDGE('',*,*,#1995,.F.);
#2737=ORIENTED_EDGE('',*,*,#1982,.T.);
#2738=ORIENTED_EDGE('',*,*,#1993,.T.);
#2739=ORIENTED_EDGE('',*,*,#1989,.T.);
#2740=ORIENTED_EDGE('',*,*,#2000,.F.);
#2741=ORIENTED_EDGE('',*,*,#1983,.T.);
#2742=ORIENTED_EDGE('',*,*,#2000,.T.);
#2743=ORIENTED_EDGE('',*,*,#1988,.T.);
#2744=ORIENTED_EDGE('',*,*,#1999,.F.);
#2745=ORIENTED_EDGE('',*,*,#1984,.T.);
#2746=ORIENTED_EDGE('',*,*,#1996,.T.);
#2747=ORIENTED_EDGE('',*,*,#1979,.T.);
#2748=ORIENTED_EDGE('',*,*,#1998,.F.);
#2749=CYLINDRICAL_SURFACE('',#3179,0.25);
#2750=CYLINDRICAL_SURFACE('',#3186,0.3);
#2751=CYLINDRICAL_SURFACE('',#3189,0.275);
#2752=CYLINDRICAL_SURFACE('',#3192,0.275);
#2753=CYLINDRICAL_SURFACE('',#3195,0.61);
#2754=CYLINDRICAL_SURFACE('',#3203,0.31);
#2755=CYLINDRICAL_SURFACE('',#3225,0.2942);
#2756=CYLINDRICAL_SURFACE('',#3238,0.275);
#2757=CYLINDRICAL_SURFACE('',#3241,0.274999999999999);
#2758=CYLINDRICAL_SURFACE('',#3246,0.300000000000001);
#2759=CYLINDRICAL_SURFACE('',#3269,0.275);
#2760=CYLINDRICAL_SURFACE('',#3272,0.31);
#2761=CYLINDRICAL_SURFACE('',#3275,0.31);
#2762=CYLINDRICAL_SURFACE('',#3278,0.6);
#2763=CYLINDRICAL_SURFACE('',#3286,0.6);
#2764=CYLINDRICAL_SURFACE('',#3288,0.6);
#2765=CYLINDRICAL_SURFACE('',#3295,0.6);
#2766=CYLINDRICAL_SURFACE('',#3297,0.31);
#2767=CYLINDRICAL_SURFACE('',#3300,0.4);
#2768=CYLINDRICAL_SURFACE('',#3306,0.31);
#2769=CYLINDRICAL_SURFACE('',#3309,0.4);
#2770=CYLINDRICAL_SURFACE('',#3315,0.21);
#2771=CYLINDRICAL_SURFACE('',#3319,0.7);
#2772=CYLINDRICAL_SURFACE('',#3339,0.425);
#2773=CYLINDRICAL_SURFACE('',#3347,0.24505);
#2774=CYLINDRICAL_SURFACE('',#3350,0.31);
#2775=CYLINDRICAL_SURFACE('',#3353,0.31);
#2776=CYLINDRICAL_SURFACE('',#3356,0.6);
#2777=CYLINDRICAL_SURFACE('',#3363,0.6);
#2778=CYLINDRICAL_SURFACE('',#3369,0.34);
#2779=CYLINDRICAL_SURFACE('',#3373,0.425);
#2780=CYLINDRICAL_SURFACE('',#3376,0.425);
#2781=CYLINDRICAL_SURFACE('',#3386,0.31);
#2782=CYLINDRICAL_SURFACE('',#3389,0.6);
#2783=CYLINDRICAL_SURFACE('',#3402,0.6);
#2784=CYLINDRICAL_SURFACE('',#3404,0.31);
#2785=CYLINDRICAL_SURFACE('',#3407,0.4);
#2786=CYLINDRICAL_SURFACE('',#3413,0.08);
#2787=CYLINDRICAL_SURFACE('',#3418,0.5);
#2788=CYLINDRICAL_SURFACE('',#3422,0.3);
#2789=CYLINDRICAL_SURFACE('',#3428,0.32);
#2790=CYLINDRICAL_SURFACE('',#3431,0.6);
#2791=CYLINDRICAL_SURFACE('',#3447,0.08);
#2792=CYLINDRICAL_SURFACE('',#3461,0.4);
#2793=CYLINDRICAL_SURFACE('',#3469,0.4);
#2794=CYLINDRICAL_SURFACE('',#3474,0.42);
#2795=CYLINDRICAL_SURFACE('',#3477,0.8);
#2796=CYLINDRICAL_SURFACE('',#3490,0.338975);
#2797=ADVANCED_FACE('',(#393),#2749,.F.);
#2798=ADVANCED_FACE('',(#394),#278,.T.);
#2799=ADVANCED_FACE('',(#395),#279,.T.);
#2800=ADVANCED_FACE('',(#396),#280,.F.);
#2801=ADVANCED_FACE('',(#397),#2750,.T.);
#2802=ADVANCED_FACE('',(#398),#281,.T.);
#2803=ADVANCED_FACE('',(#399),#2751,.F.);
#2804=ADVANCED_FACE('',(#400),#2752,.F.);
#2805=ADVANCED_FACE('',(#401),#2753,.F.);
#2806=ADVANCED_FACE('',(#402),#282,.F.);
#2807=ADVANCED_FACE('',(#403,#222),#283,.T.);
#2808=ADVANCED_FACE('',(#404,#223),#284,.T.);
#2809=ADVANCED_FACE('',(#405),#285,.T.);
#2810=ADVANCED_FACE('',(#406),#286,.T.);
#2811=ADVANCED_FACE('',(#407),#2754,.F.);
#2812=ADVANCED_FACE('',(#408,#224),#287,.F.);
#2813=ADVANCED_FACE('',(#409),#288,.T.);
#2814=ADVANCED_FACE('',(#410),#289,.T.);
#2815=ADVANCED_FACE('',(#411),#290,.T.);
#2816=ADVANCED_FACE('',(#412,#225),#291,.T.);
#2817=ADVANCED_FACE('',(#413,#226),#292,.F.);
#2818=ADVANCED_FACE('',(#414),#293,.T.);
#2819=ADVANCED_FACE('',(#415),#294,.T.);
#2820=ADVANCED_FACE('',(#416),#295,.T.);
#2821=ADVANCED_FACE('',(#417,#227),#296,.T.);
#2822=ADVANCED_FACE('',(#418),#297,.T.);
#2823=ADVANCED_FACE('',(#419),#298,.T.);
#2824=ADVANCED_FACE('',(#420),#299,.T.);
#2825=ADVANCED_FACE('',(#421),#300,.T.);
#2826=ADVANCED_FACE('',(#422,#228,#229,#230,#231,#232,#233),#301,.T.);
#2827=ADVANCED_FACE('',(#423,#234,#235),#302,.F.);
#2828=ADVANCED_FACE('',(#424),#303,.F.);
#2829=ADVANCED_FACE('',(#425),#2755,.T.);
#2830=ADVANCED_FACE('',(#426),#147,.T.);
#2831=ADVANCED_FACE('',(#427),#304,.T.);
#2832=ADVANCED_FACE('',(#428),#305,.T.);
#2833=ADVANCED_FACE('',(#429),#306,.T.);
#2834=ADVANCED_FACE('',(#430),#307,.T.);
#2835=ADVANCED_FACE('',(#431),#308,.T.);
#2836=ADVANCED_FACE('',(#432),#309,.T.);
#2837=ADVANCED_FACE('',(#433),#310,.T.);
#2838=ADVANCED_FACE('',(#434,#236),#311,.F.);
#2839=ADVANCED_FACE('',(#435),#2756,.F.);
#2840=ADVANCED_FACE('',(#436),#2757,.F.);
#2841=ADVANCED_FACE('',(#437),#312,.F.);
#2842=ADVANCED_FACE('',(#438),#2758,.T.);
#2843=ADVANCED_FACE('',(#439),#313,.T.);
#2844=ADVANCED_FACE('',(#440),#314,.T.);
#2845=ADVANCED_FACE('',(#441),#315,.T.);
#2846=ADVANCED_FACE('',(#442),#316,.T.);
#2847=ADVANCED_FACE('',(#443),#317,.T.);
#2848=ADVANCED_FACE('',(#444),#318,.T.);
#2849=ADVANCED_FACE('',(#445),#319,.F.);
#2850=ADVANCED_FACE('',(#446),#320,.T.);
#2851=ADVANCED_FACE('',(#447),#321,.T.);
#2852=ADVANCED_FACE('',(#448),#322,.T.);
#2853=ADVANCED_FACE('',(#449),#323,.T.);
#2854=ADVANCED_FACE('',(#450),#324,.T.);
#2855=ADVANCED_FACE('',(#451),#325,.T.);
#2856=ADVANCED_FACE('',(#452,#237,#238,#239,#240),#326,.T.);
#2857=ADVANCED_FACE('',(#453,#241,#242),#327,.F.);
#2858=ADVANCED_FACE('',(#454),#2759,.F.);
#2859=ADVANCED_FACE('',(#455),#2760,.F.);
#2860=ADVANCED_FACE('',(#456),#2761,.F.);
#2861=ADVANCED_FACE('',(#457),#2762,.T.);
#2862=ADVANCED_FACE('',(#458,#243,#244,#245),#328,.F.);
#2863=ADVANCED_FACE('',(#459),#329,.T.);
#2864=ADVANCED_FACE('',(#460),#2763,.T.);
#2865=ADVANCED_FACE('',(#461),#2764,.T.);
#2866=ADVANCED_FACE('',(#462,#246,#247,#248),#330,.T.);
#2867=ADVANCED_FACE('',(#463),#331,.T.);
#2868=ADVANCED_FACE('',(#464),#332,.T.);
#2869=ADVANCED_FACE('',(#465),#333,.T.);
#2870=ADVANCED_FACE('',(#466),#2765,.T.);
#2871=ADVANCED_FACE('',(#467),#2766,.F.);
#2872=ADVANCED_FACE('',(#468),#2767,.T.);
#2873=ADVANCED_FACE('',(#469,#249),#334,.T.);
#2874=ADVANCED_FACE('',(#470,#250),#335,.F.);
#2875=ADVANCED_FACE('',(#471),#2768,.F.);
#2876=ADVANCED_FACE('',(#472),#2769,.T.);
#2877=ADVANCED_FACE('',(#473,#251),#336,.T.);
#2878=ADVANCED_FACE('',(#474,#252),#337,.F.);
#2879=ADVANCED_FACE('',(#475),#2770,.F.);
#2880=ADVANCED_FACE('',(#476),#338,.T.);
#2881=ADVANCED_FACE('',(#477),#2771,.T.);
#2882=ADVANCED_FACE('',(#478,#253),#339,.T.);
#2883=ADVANCED_FACE('',(#479),#340,.F.);
#2884=ADVANCED_FACE('',(#480),#341,.F.);
#2885=ADVANCED_FACE('',(#481),#342,.F.);
#2886=ADVANCED_FACE('',(#482),#343,.F.);
#2887=ADVANCED_FACE('',(#483),#344,.F.);
#2888=ADVANCED_FACE('',(#484),#345,.F.);
#2889=ADVANCED_FACE('',(#485),#346,.F.);
#2890=ADVANCED_FACE('',(#486),#347,.F.);
#2891=ADVANCED_FACE('',(#487),#348,.F.);
#2892=ADVANCED_FACE('',(#488),#349,.F.);
#2893=ADVANCED_FACE('',(#489),#350,.T.);
#2894=ADVANCED_FACE('',(#490),#148,.T.);
#2895=ADVANCED_FACE('',(#491),#2772,.T.);
#2896=ADVANCED_FACE('',(#492),#149,.T.);
#2897=ADVANCED_FACE('',(#493,#254),#351,.T.);
#2898=ADVANCED_FACE('',(#494),#150,.T.);
#2899=ADVANCED_FACE('',(#495),#2773,.T.);
#2900=ADVANCED_FACE('',(#496),#2774,.F.);
#2901=ADVANCED_FACE('',(#497),#2775,.F.);
#2902=ADVANCED_FACE('',(#498),#2776,.T.);
#2903=ADVANCED_FACE('',(#499),#352,.T.);
#2904=ADVANCED_FACE('',(#500,#255,#256),#353,.F.);
#2905=ADVANCED_FACE('',(#501),#354,.T.);
#2906=ADVANCED_FACE('',(#502),#2777,.T.);
#2907=ADVANCED_FACE('',(#503,#257,#258),#355,.T.);
#2908=ADVANCED_FACE('',(#504),#2778,.F.);
#2909=ADVANCED_FACE('',(#505),#356,.T.);
#2910=ADVANCED_FACE('',(#506),#2779,.F.);
#2911=ADVANCED_FACE('',(#507),#2780,.F.);
#2912=ADVANCED_FACE('',(#508,#259,#260,#261),#357,.F.);
#2913=ADVANCED_FACE('',(#509),#358,.T.);
#2914=ADVANCED_FACE('',(#510),#359,.T.);
#2915=ADVANCED_FACE('',(#511),#360,.T.);
#2916=ADVANCED_FACE('',(#512),#361,.T.);
#2917=ADVANCED_FACE('',(#513,#262,#263,#264),#362,.T.);
#2918=ADVANCED_FACE('',(#514),#2781,.F.);
#2919=ADVANCED_FACE('',(#515),#2782,.T.);
#2920=ADVANCED_FACE('',(#516,#265),#363,.F.);
#2921=ADVANCED_FACE('',(#517),#364,.T.);
#2922=ADVANCED_FACE('',(#518),#365,.F.);
#2923=ADVANCED_FACE('',(#519),#366,.T.);
#2924=ADVANCED_FACE('',(#520),#367,.T.);
#2925=ADVANCED_FACE('',(#521),#368,.T.);
#2926=ADVANCED_FACE('',(#522,#266),#369,.T.);
#2927=ADVANCED_FACE('',(#523),#370,.F.);
#2928=ADVANCED_FACE('',(#524),#2783,.T.);
#2929=ADVANCED_FACE('',(#525),#2784,.F.);
#2930=ADVANCED_FACE('',(#526),#2785,.T.);
#2931=ADVANCED_FACE('',(#527,#267),#371,.T.);
#2932=ADVANCED_FACE('',(#528,#268),#372,.F.);
#2933=ADVANCED_FACE('',(#529),#2786,.F.);
#2934=ADVANCED_FACE('',(#530),#373,.T.);
#2935=ADVANCED_FACE('',(#531),#151,.T.);
#2936=ADVANCED_FACE('',(#532),#2787,.T.);
#2937=ADVANCED_FACE('',(#533,#269),#374,.T.);
#2938=ADVANCED_FACE('',(#534,#270),#2788,.T.);
#2939=ADVANCED_FACE('',(#535),#152,.T.);
#2940=ADVANCED_FACE('',(#536),#375,.T.);
#2941=ADVANCED_FACE('',(#537),#2789,.F.);
#2942=ADVANCED_FACE('',(#538),#2790,.T.);
#2943=ADVANCED_FACE('',(#539,#271),#376,.T.);
#2944=ADVANCED_FACE('',(#540,#272),#377,.F.);
#2945=ADVANCED_FACE('',(#541,#273),#11,.T.);
#2946=ADVANCED_FACE('',(#542),#378,.F.);
#2947=ADVANCED_FACE('',(#543),#379,.T.);
#2948=ADVANCED_FACE('',(#544),#2791,.T.);
#2949=ADVANCED_FACE('',(#545),#380,.F.);
#2950=ADVANCED_FACE('',(#546),#2792,.T.);
#2951=ADVANCED_FACE('',(#547),#12,.T.);
#2952=ADVANCED_FACE('',(#548),#2793,.T.);
#2953=ADVANCED_FACE('',(#549),#381,.T.);
#2954=ADVANCED_FACE('',(#550),#382,.F.);
#2955=ADVANCED_FACE('',(#551),#2794,.F.);
#2956=ADVANCED_FACE('',(#552),#2795,.T.);
#2957=ADVANCED_FACE('',(#553,#274),#383,.T.);
#2958=ADVANCED_FACE('',(#554,#275),#384,.F.);
#2959=ADVANCED_FACE('',(#555),#153,.T.);
#2960=ADVANCED_FACE('',(#556),#154,.T.);
#2961=ADVANCED_FACE('',(#557),#385,.T.);
#2962=ADVANCED_FACE('',(#558),#386,.T.);
#2963=ADVANCED_FACE('',(#559),#387,.T.);
#2964=ADVANCED_FACE('',(#560),#2796,.F.);
#2965=ADVANCED_FACE('',(#561),#388,.T.);
#2966=ADVANCED_FACE('',(#562),#389,.T.);
#2967=ADVANCED_FACE('',(#563),#390,.T.);
#2968=ADVANCED_FACE('',(#564,#276),#391,.T.);
#2969=ADVANCED_FACE('',(#565,#277),#392,.F.);
#2970=CLOSED_SHELL('',(#2797,#2798,#2799,#2800,#2801,#2802,#2803,#2804,
#2805,#2806,#2807,#2808,#2809,#2810,#2811,#2812,#2813,#2814,#2815,#2816,
#2817,#2818,#2819,#2820,#2821,#2822,#2823,#2824,#2825,#2826,#2827));
#2971=CLOSED_SHELL('',(#2828,#2829,#2830,#2831,#2832,#2833,#2834,#2835,
#2836,#2837,#2838));
#2972=CLOSED_SHELL('',(#2839,#2840,#2841,#2842,#2843,#2844,#2845,#2846,
#2847,#2848,#2849,#2850,#2851,#2852,#2853,#2854,#2855,#2856,#2857));
#2973=CLOSED_SHELL('',(#2858,#2859,#2860,#2861,#2862,#2863,#2864,#2865,
#2866,#2867,#2868,#2869,#2870));
#2974=CLOSED_SHELL('',(#2871,#2872,#2873,#2874));
#2975=CLOSED_SHELL('',(#2875,#2876,#2877,#2878));
#2976=CLOSED_SHELL('',(#2879,#2880,#2881,#2882,#2883));
#2977=CLOSED_SHELL('',(#2884,#2885,#2886,#2887,#2888,#2889,#2890,#2891));
#2978=CLOSED_SHELL('',(#2892,#2893,#2894,#2895,#2896,#2897,#2898,#2899));
#2979=CLOSED_SHELL('',(#2900,#2901,#2902,#2903,#2904,#2905,#2906,#2907));
#2980=CLOSED_SHELL('',(#2908,#2909,#2910,#2911,#2912,#2913,#2914,#2915,
#2916,#2917,#2918,#2919,#2920,#2921,#2922,#2923,#2924,#2925,#2926,#2927,
#2928));
#2981=CLOSED_SHELL('',(#2929,#2930,#2931,#2932));
#2982=CLOSED_SHELL('',(#2933,#2934,#2935,#2936,#2937,#2938,#2939,#2940));
#2983=CLOSED_SHELL('',(#2941,#2942,#2943,#2944));
#2984=CLOSED_SHELL('',(#2945,#2946,#2947,#2948,#2949));
#2985=CLOSED_SHELL('',(#2950,#2951,#2952,#2953,#2954));
#2986=CLOSED_SHELL('',(#2955,#2956,#2957,#2958));
#2987=CLOSED_SHELL('',(#2959,#2960,#2961,#2962,#2963,#2964,#2965,#2966,
#2967,#2968,#2969));
#2988=DERIVED_UNIT_ELEMENT(#3022,1.);
#2989=DERIVED_UNIT_ELEMENT(#5460,-3.);
#2990=DERIVED_UNIT_ELEMENT(#3022,1.);
#2991=DERIVED_UNIT_ELEMENT(#5460,-3.);
#2992=DERIVED_UNIT_ELEMENT(#3022,1.);
#2993=DERIVED_UNIT_ELEMENT(#5460,-3.);
#2994=DERIVED_UNIT_ELEMENT(#3022,1.);
#2995=DERIVED_UNIT_ELEMENT(#5460,-3.);
#2996=DERIVED_UNIT_ELEMENT(#3022,1.);
#2997=DERIVED_UNIT_ELEMENT(#5460,-3.);
#2998=DERIVED_UNIT_ELEMENT(#3022,1.);
#2999=DERIVED_UNIT_ELEMENT(#5460,-3.);
#3000=DERIVED_UNIT_ELEMENT(#3022,1.);
#3001=DERIVED_UNIT_ELEMENT(#5460,-3.);
#3002=DERIVED_UNIT_ELEMENT(#3022,1.);
#3003=DERIVED_UNIT_ELEMENT(#5460,-3.);
#3004=DERIVED_UNIT_ELEMENT(#3022,1.);
#3005=DERIVED_UNIT_ELEMENT(#5460,-3.);
#3006=DERIVED_UNIT_ELEMENT(#3022,1.);
#3007=DERIVED_UNIT_ELEMENT(#5460,-3.);
#3008=DERIVED_UNIT_ELEMENT(#3022,1.);
#3009=DERIVED_UNIT_ELEMENT(#5460,-3.);
#3010=DERIVED_UNIT_ELEMENT(#3022,1.);
#3011=DERIVED_UNIT_ELEMENT(#5460,-3.);
#3012=DERIVED_UNIT_ELEMENT(#3022,1.);
#3013=DERIVED_UNIT_ELEMENT(#5460,-3.);
#3014=DERIVED_UNIT_ELEMENT(#3022,1.);
#3015=DERIVED_UNIT_ELEMENT(#5460,-3.);
#3016=DERIVED_UNIT_ELEMENT(#3022,1.);
#3017=DERIVED_UNIT_ELEMENT(#5460,-3.);
#3018=DERIVED_UNIT_ELEMENT(#3022,1.);
#3019=DERIVED_UNIT_ELEMENT(#5460,-3.);
#3020=DERIVED_UNIT_ELEMENT(#3022,1.);
#3021=DERIVED_UNIT_ELEMENT(#5460,-3.);
#3022=(
MASS_UNIT()
NAMED_UNIT(*)
SI_UNIT(.KILO.,.GRAM.)
);
#3023=DERIVED_UNIT((#2988,#2989));
#3024=DERIVED_UNIT((#2990,#2991));
#3025=DERIVED_UNIT((#2992,#2993));
#3026=DERIVED_UNIT((#2994,#2995));
#3027=DERIVED_UNIT((#2996,#2997));
#3028=DERIVED_UNIT((#2998,#2999));
#3029=DERIVED_UNIT((#3000,#3001));
#3030=DERIVED_UNIT((#3002,#3003));
#3031=DERIVED_UNIT((#3004,#3005));
#3032=DERIVED_UNIT((#3006,#3007));
#3033=DERIVED_UNIT((#3008,#3009));
#3034=DERIVED_UNIT((#3010,#3011));
#3035=DERIVED_UNIT((#3012,#3013));
#3036=DERIVED_UNIT((#3014,#3015));
#3037=DERIVED_UNIT((#3016,#3017));
#3038=DERIVED_UNIT((#3018,#3019));
#3039=DERIVED_UNIT((#3020,#3021));
#3040=MEASURE_REPRESENTATION_ITEM('density measure',
POSITIVE_RATIO_MEASURE(7850.),#3023);
#3041=MEASURE_REPRESENTATION_ITEM('density measure',
POSITIVE_RATIO_MEASURE(7850.),#3024);
#3042=MEASURE_REPRESENTATION_ITEM('density measure',
POSITIVE_RATIO_MEASURE(7850.),#3025);
#3043=MEASURE_REPRESENTATION_ITEM('density measure',
POSITIVE_RATIO_MEASURE(7850.),#3026);
#3044=MEASURE_REPRESENTATION_ITEM('density measure',
POSITIVE_RATIO_MEASURE(7850.),#3027);
#3045=MEASURE_REPRESENTATION_ITEM('density measure',
POSITIVE_RATIO_MEASURE(7850.),#3028);
#3046=MEASURE_REPRESENTATION_ITEM('density measure',
POSITIVE_RATIO_MEASURE(7850.),#3029);
#3047=MEASURE_REPRESENTATION_ITEM('density measure',
POSITIVE_RATIO_MEASURE(7850.),#3030);
#3048=MEASURE_REPRESENTATION_ITEM('density measure',
POSITIVE_RATIO_MEASURE(7850.),#3031);
#3049=MEASURE_REPRESENTATION_ITEM('density measure',
POSITIVE_RATIO_MEASURE(7850.),#3032);
#3050=MEASURE_REPRESENTATION_ITEM('density measure',
POSITIVE_RATIO_MEASURE(7850.),#3033);
#3051=MEASURE_REPRESENTATION_ITEM('density measure',
POSITIVE_RATIO_MEASURE(7850.),#3034);
#3052=MEASURE_REPRESENTATION_ITEM('density measure',
POSITIVE_RATIO_MEASURE(7850.),#3035);
#3053=MEASURE_REPRESENTATION_ITEM('density measure',
POSITIVE_RATIO_MEASURE(7850.),#3036);
#3054=MEASURE_REPRESENTATION_ITEM('density measure',
POSITIVE_RATIO_MEASURE(7850.),#3037);
#3055=MEASURE_REPRESENTATION_ITEM('density measure',
POSITIVE_RATIO_MEASURE(7850.),#3038);
#3056=MEASURE_REPRESENTATION_ITEM('density measure',
POSITIVE_RATIO_MEASURE(7850.),#3039);
#3057=PROPERTY_DEFINITION_REPRESENTATION(#3142,#3091);
#3058=PROPERTY_DEFINITION_REPRESENTATION(#3143,#3092);
#3059=PROPERTY_DEFINITION_REPRESENTATION(#3144,#3093);
#3060=PROPERTY_DEFINITION_REPRESENTATION(#3145,#3094);
#3061=PROPERTY_DEFINITION_REPRESENTATION(#3146,#3095);
#3062=PROPERTY_DEFINITION_REPRESENTATION(#3147,#3096);
#3063=PROPERTY_DEFINITION_REPRESENTATION(#3148,#3097);
#3064=PROPERTY_DEFINITION_REPRESENTATION(#3149,#3098);
#3065=PROPERTY_DEFINITION_REPRESENTATION(#3150,#3099);
#3066=PROPERTY_DEFINITION_REPRESENTATION(#3151,#3100);
#3067=PROPERTY_DEFINITION_REPRESENTATION(#3152,#3101);
#3068=PROPERTY_DEFINITION_REPRESENTATION(#3153,#3102);
#3069=PROPERTY_DEFINITION_REPRESENTATION(#3154,#3103);
#3070=PROPERTY_DEFINITION_REPRESENTATION(#3155,#3104);
#3071=PROPERTY_DEFINITION_REPRESENTATION(#3156,#3105);
#3072=PROPERTY_DEFINITION_REPRESENTATION(#3157,#3106);
#3073=PROPERTY_DEFINITION_REPRESENTATION(#3158,#3107);
#3074=PROPERTY_DEFINITION_REPRESENTATION(#3159,#3108);
#3075=PROPERTY_DEFINITION_REPRESENTATION(#3160,#3109);
#3076=PROPERTY_DEFINITION_REPRESENTATION(#3161,#3110);
#3077=PROPERTY_DEFINITION_REPRESENTATION(#3162,#3111);
#3078=PROPERTY_DEFINITION_REPRESENTATION(#3163,#3112);
#3079=PROPERTY_DEFINITION_REPRESENTATION(#3164,#3113);
#3080=PROPERTY_DEFINITION_REPRESENTATION(#3165,#3114);
#3081=PROPERTY_DEFINITION_REPRESENTATION(#3166,#3115);
#3082=PROPERTY_DEFINITION_REPRESENTATION(#3167,#3116);
#3083=PROPERTY_DEFINITION_REPRESENTATION(#3168,#3117);
#3084=PROPERTY_DEFINITION_REPRESENTATION(#3169,#3118);
#3085=PROPERTY_DEFINITION_REPRESENTATION(#3170,#3119);
#3086=PROPERTY_DEFINITION_REPRESENTATION(#3171,#3120);
#3087=PROPERTY_DEFINITION_REPRESENTATION(#3172,#3121);
#3088=PROPERTY_DEFINITION_REPRESENTATION(#3173,#3122);
#3089=PROPERTY_DEFINITION_REPRESENTATION(#3174,#3123);
#3090=PROPERTY_DEFINITION_REPRESENTATION(#3175,#3124);
#3091=REPRESENTATION('material name',(#3125),#5438);
#3092=REPRESENTATION('density',(#3040),#5438);
#3093=REPRESENTATION('material name',(#3126),#5439);
#3094=REPRESENTATION('density',(#3041),#5439);
#3095=REPRESENTATION('material name',(#3127),#5440);
#3096=REPRESENTATION('density',(#3042),#5440);
#3097=REPRESENTATION('material name',(#3128),#5442);
#3098=REPRESENTATION('density',(#3043),#5442);
#3099=REPRESENTATION('material name',(#3129),#5443);
#3100=REPRESENTATION('density',(#3044),#5443);
#3101=REPRESENTATION('material name',(#3130),#5444);
#3102=REPRESENTATION('density',(#3045),#5444);
#3103=REPRESENTATION('material name',(#3131),#5445);
#3104=REPRESENTATION('density',(#3046),#5445);
#3105=REPRESENTATION('material name',(#3132),#5446);
#3106=REPRESENTATION('density',(#3047),#5446);
#3107=REPRESENTATION('material name',(#3133),#5448);
#3108=REPRESENTATION('density',(#3048),#5448);
#3109=REPRESENTATION('material name',(#3134),#5450);
#3110=REPRESENTATION('density',(#3049),#5450);
#3111=REPRESENTATION('material name',(#3135),#5451);
#3112=REPRESENTATION('density',(#3050),#5451);
#3113=REPRESENTATION('material name',(#3136),#5452);
#3114=REPRESENTATION('density',(#3051),#5452);
#3115=REPRESENTATION('material name',(#3137),#5453);
#3116=REPRESENTATION('density',(#3052),#5453);
#3117=REPRESENTATION('material name',(#3138),#5454);
#3118=REPRESENTATION('density',(#3053),#5454);
#3119=REPRESENTATION('material name',(#3139),#5455);
#3120=REPRESENTATION('density',(#3054),#5455);
#3121=REPRESENTATION('material name',(#3140),#5456);
#3122=REPRESENTATION('density',(#3055),#5456);
#3123=REPRESENTATION('material name',(#3141),#5457);
#3124=REPRESENTATION('density',(#3056),#5457);
#3125=DESCRIPTIVE_REPRESENTATION_ITEM('Steel','Steel');
#3126=DESCRIPTIVE_REPRESENTATION_ITEM('Steel','Steel');
#3127=DESCRIPTIVE_REPRESENTATION_ITEM('Steel','Steel');
#3128=DESCRIPTIVE_REPRESENTATION_ITEM('Steel','Steel');
#3129=DESCRIPTIVE_REPRESENTATION_ITEM('Steel','Steel');
#3130=DESCRIPTIVE_REPRESENTATION_ITEM('Steel','Steel');
#3131=DESCRIPTIVE_REPRESENTATION_ITEM('Steel','Steel');
#3132=DESCRIPTIVE_REPRESENTATION_ITEM('Steel','Steel');
#3133=DESCRIPTIVE_REPRESENTATION_ITEM('Steel','Steel');
#3134=DESCRIPTIVE_REPRESENTATION_ITEM('Steel','Steel');
#3135=DESCRIPTIVE_REPRESENTATION_ITEM('Steel','Steel');
#3136=DESCRIPTIVE_REPRESENTATION_ITEM('Steel','Steel');
#3137=DESCRIPTIVE_REPRESENTATION_ITEM('Steel','Steel');
#3138=DESCRIPTIVE_REPRESENTATION_ITEM('Steel','Steel');
#3139=DESCRIPTIVE_REPRESENTATION_ITEM('Steel','Steel');
#3140=DESCRIPTIVE_REPRESENTATION_ITEM('Steel','Steel');
#3141=DESCRIPTIVE_REPRESENTATION_ITEM('Steel','Steel');
#3142=PROPERTY_DEFINITION('material property','material name',#5559);
#3143=PROPERTY_DEFINITION('material property','density of part',#5559);
#3144=PROPERTY_DEFINITION('material property','material name',#5560);
#3145=PROPERTY_DEFINITION('material property','density of part',#5560);
#3146=PROPERTY_DEFINITION('material property','material name',#5561);
#3147=PROPERTY_DEFINITION('material property','density of part',#5561);
#3148=PROPERTY_DEFINITION('material property','material name',#5563);
#3149=PROPERTY_DEFINITION('material property','density of part',#5563);
#3150=PROPERTY_DEFINITION('material property','material name',#5564);
#3151=PROPERTY_DEFINITION('material property','density of part',#5564);
#3152=PROPERTY_DEFINITION('material property','material name',#5565);
#3153=PROPERTY_DEFINITION('material property','density of part',#5565);
#3154=PROPERTY_DEFINITION('material property','material name',#5566);
#3155=PROPERTY_DEFINITION('material property','density of part',#5566);
#3156=PROPERTY_DEFINITION('material property','material name',#5567);
#3157=PROPERTY_DEFINITION('material property','density of part',#5567);
#3158=PROPERTY_DEFINITION('material property','material name',#5569);
#3159=PROPERTY_DEFINITION('material property','density of part',#5569);
#3160=PROPERTY_DEFINITION('material property','material name',#5571);
#3161=PROPERTY_DEFINITION('material property','density of part',#5571);
#3162=PROPERTY_DEFINITION('material property','material name',#5572);
#3163=PROPERTY_DEFINITION('material property','density of part',#5572);
#3164=PROPERTY_DEFINITION('material property','material name',#5573);
#3165=PROPERTY_DEFINITION('material property','density of part',#5573);
#3166=PROPERTY_DEFINITION('material property','material name',#5574);
#3167=PROPERTY_DEFINITION('material property','density of part',#5574);
#3168=PROPERTY_DEFINITION('material property','material name',#5575);
#3169=PROPERTY_DEFINITION('material property','density of part',#5575);
#3170=PROPERTY_DEFINITION('material property','material name',#5576);
#3171=PROPERTY_DEFINITION('material property','density of part',#5576);
#3172=PROPERTY_DEFINITION('material property','material name',#5577);
#3173=PROPERTY_DEFINITION('material property','density of part',#5577);
#3174=PROPERTY_DEFINITION('material property','material name',#5578);
#3175=PROPERTY_DEFINITION('material property','density of part',#5578);
#3176=AXIS2_PLACEMENT_3D('',#4418,#3511,#3512);
#3177=AXIS2_PLACEMENT_3D('',#4419,#3513,#3514);
#3178=AXIS2_PLACEMENT_3D('',#4420,#3515,#3516);
#3179=AXIS2_PLACEMENT_3D('',#4421,#3517,#3518);
#3180=AXIS2_PLACEMENT_3D('',#4423,#3519,#3520);
#3181=AXIS2_PLACEMENT_3D('',#4426,#3522,#3523);
#3182=AXIS2_PLACEMENT_3D('',#4427,#3524,#3525);
#3183=AXIS2_PLACEMENT_3D('',#4436,#3530,#3531);
#3184=AXIS2_PLACEMENT_3D('',#4445,#3536,#3537);
#3185=AXIS2_PLACEMENT_3D('',#4446,#3538,#3539);
#3186=AXIS2_PLACEMENT_3D('',#4448,#3541,#3542);
#3187=AXIS2_PLACEMENT_3D('',#4449,#3543,#3544);
#3188=AXIS2_PLACEMENT_3D('',#4450,#3545,#3546);
#3189=AXIS2_PLACEMENT_3D('',#4452,#3548,#3549);
#3190=AXIS2_PLACEMENT_3D('',#4454,#3550,#3551);
#3191=AXIS2_PLACEMENT_3D('',#4457,#3553,#3554);
#3192=AXIS2_PLACEMENT_3D('',#4458,#3555,#3556);
#3193=AXIS2_PLACEMENT_3D('',#4460,#3557,#3558);
#3194=AXIS2_PLACEMENT_3D('',#4463,#3560,#3561);
#3195=AXIS2_PLACEMENT_3D('',#4464,#3562,#3563);
#3196=AXIS2_PLACEMENT_3D('',#4466,#3564,#3565);
#3197=AXIS2_PLACEMENT_3D('',#4469,#3567,#3568);
#3198=AXIS2_PLACEMENT_3D('',#4470,#3569,#3570);
#3199=AXIS2_PLACEMENT_3D('',#4479,#3575,#3576);
#3200=AXIS2_PLACEMENT_3D('',#4485,#3580,#3581);
#3201=AXIS2_PLACEMENT_3D('',#4491,#3585,#3586);
#3202=AXIS2_PLACEMENT_3D('',#4493,#3588,#3589);
#3203=AXIS2_PLACEMENT_3D('',#4495,#3591,#3592);
#3204=AXIS2_PLACEMENT_3D('',#4497,#3593,#3594);
#3205=AXIS2_PLACEMENT_3D('',#4500,#3596,#3597);
#3206=AXIS2_PLACEMENT_3D('',#4501,#3598,#3599);
#3207=AXIS2_PLACEMENT_3D('',#4510,#3604,#3605);
#3208=AXIS2_PLACEMENT_3D('',#4516,#3609,#3610);
#3209=AXIS2_PLACEMENT_3D('',#4522,#3614,#3615);
#3210=AXIS2_PLACEMENT_3D('',#4524,#3617,#3618);
#3211=AXIS2_PLACEMENT_3D('',#4526,#3620,#3621);
#3212=AXIS2_PLACEMENT_3D('',#4535,#3626,#3627);
#3213=AXIS2_PLACEMENT_3D('',#4541,#3631,#3632);
#3214=AXIS2_PLACEMENT_3D('',#4547,#3636,#3637);
#3215=AXIS2_PLACEMENT_3D('',#4549,#3639,#3640);
#3216=AXIS2_PLACEMENT_3D('',#4551,#3642,#3643);
#3217=AXIS2_PLACEMENT_3D('',#4560,#3648,#3649);
#3218=AXIS2_PLACEMENT_3D('',#4566,#3653,#3654);
#3219=AXIS2_PLACEMENT_3D('',#4572,#3658,#3659);
#3220=AXIS2_PLACEMENT_3D('',#4575,#3662,#3663);
#3221=AXIS2_PLACEMENT_3D('',#4576,#3664,#3665);
#3222=AXIS2_PLACEMENT_3D('',#4577,#3666,#3667);
#3223=AXIS2_PLACEMENT_3D('',#4578,#3668,#3669);
#3224=AXIS2_PLACEMENT_3D('',#4580,#3670,#3671);
#3225=AXIS2_PLACEMENT_3D('',#4581,#3672,#3673);
#3226=AXIS2_PLACEMENT_3D('',#4584,#3675,#3676);
#3227=AXIS2_PLACEMENT_3D('',#4585,#3677,#3678);
#3228=AXIS2_PLACEMENT_3D('',#4587,#3679,#3680);
#3229=AXIS2_PLACEMENT_3D('',#4613,#3682,#3683);
#3230=AXIS2_PLACEMENT_3D('',#4619,#3687,#3688);
#3231=AXIS2_PLACEMENT_3D('',#4623,#3691,#3692);
#3232=AXIS2_PLACEMENT_3D('',#4627,#3695,#3696);
#3233=AXIS2_PLACEMENT_3D('',#4631,#3699,#3700);
#3234=AXIS2_PLACEMENT_3D('',#4635,#3703,#3704);
#3235=AXIS2_PLACEMENT_3D('',#4637,#3706,#3707);
#3236=AXIS2_PLACEMENT_3D('',#4638,#3708,#3709);
#3237=AXIS2_PLACEMENT_3D('',#4639,#3710,#3711);
#3238=AXIS2_PLACEMENT_3D('',#4640,#3712,#3713);
#3239=AXIS2_PLACEMENT_3D('',#4642,#3714,#3715);
#3240=AXIS2_PLACEMENT_3D('',#4645,#3717,#3718);
#3241=AXIS2_PLACEMENT_3D('',#4646,#3719,#3720);
#3242=AXIS2_PLACEMENT_3D('',#4648,#3721,#3722);
#3243=AXIS2_PLACEMENT_3D('',#4651,#3724,#3725);
#3244=AXIS2_PLACEMENT_3D('',#4652,#3726,#3727);
#3245=AXIS2_PLACEMENT_3D('',#4655,#3728,#3729);
#3246=AXIS2_PLACEMENT_3D('',#4663,#3734,#3735);
#3247=AXIS2_PLACEMENT_3D('',#4669,#3738,#3739);
#3248=AXIS2_PLACEMENT_3D('',#4673,#3741,#3742);
#3249=AXIS2_PLACEMENT_3D('',#4677,#3744,#3745);
#3250=AXIS2_PLACEMENT_3D('',#4680,#3747,#3748);
#3251=AXIS2_PLACEMENT_3D('',#4681,#3749,#3750);
#3252=AXIS2_PLACEMENT_3D('',#4682,#3751,#3752);
#3253=AXIS2_PLACEMENT_3D('',#4690,#3757,#3758);
#3254=AXIS2_PLACEMENT_3D('',#4692,#3760,#3761);
#3255=AXIS2_PLACEMENT_3D('',#4694,#3763,#3764);
#3256=AXIS2_PLACEMENT_3D('',#4696,#3766,#3767);
#3257=AXIS2_PLACEMENT_3D('',#4704,#3772,#3773);
#3258=AXIS2_PLACEMENT_3D('',#4708,#3776,#3777);
#3259=AXIS2_PLACEMENT_3D('',#4714,#3781,#3782);
#3260=AXIS2_PLACEMENT_3D('',#4716,#3784,#3785);
#3261=AXIS2_PLACEMENT_3D('',#4718,#3787,#3788);
#3262=AXIS2_PLACEMENT_3D('',#4727,#3793,#3794);
#3263=AXIS2_PLACEMENT_3D('',#4733,#3798,#3799);
#3264=AXIS2_PLACEMENT_3D('',#4739,#3803,#3804);
#3265=AXIS2_PLACEMENT_3D('',#4742,#3807,#3808);
#3266=AXIS2_PLACEMENT_3D('',#4743,#3809,#3810);
#3267=AXIS2_PLACEMENT_3D('',#4744,#3811,#3812);
#3268=AXIS2_PLACEMENT_3D('',#4745,#3813,#3814);
#3269=AXIS2_PLACEMENT_3D('',#4746,#3815,#3816);
#3270=AXIS2_PLACEMENT_3D('',#4748,#3817,#3818);
#3271=AXIS2_PLACEMENT_3D('',#4751,#3820,#3821);
#3272=AXIS2_PLACEMENT_3D('',#4752,#3822,#3823);
#3273=AXIS2_PLACEMENT_3D('',#4754,#3824,#3825);
#3274=AXIS2_PLACEMENT_3D('',#4757,#3827,#3828);
#3275=AXIS2_PLACEMENT_3D('',#4758,#3829,#3830);
#3276=AXIS2_PLACEMENT_3D('',#4760,#3831,#3832);
#3277=AXIS2_PLACEMENT_3D('',#4763,#3834,#3835);
#3278=AXIS2_PLACEMENT_3D('',#4764,#3836,#3837);
#3279=AXIS2_PLACEMENT_3D('',#4769,#3839,#3840);
#3280=AXIS2_PLACEMENT_3D('',#4772,#3842,#3843);
#3281=AXIS2_PLACEMENT_3D('',#4773,#3844,#3845);
#3282=AXIS2_PLACEMENT_3D('',#4777,#3847,#3848);
#3283=AXIS2_PLACEMENT_3D('',#4781,#3850,#3851);
#3284=AXIS2_PLACEMENT_3D('',#4785,#3853,#3854);
#3285=AXIS2_PLACEMENT_3D('',#4787,#3856,#3857);
#3286=AXIS2_PLACEMENT_3D('',#4791,#3860,#3861);
#3287=AXIS2_PLACEMENT_3D('',#4793,#3862,#3863);
#3288=AXIS2_PLACEMENT_3D('',#4795,#3865,#3866);
#3289=AXIS2_PLACEMENT_3D('',#4800,#3869,#3870);
#3290=AXIS2_PLACEMENT_3D('',#4801,#3871,#3872);
#3291=AXIS2_PLACEMENT_3D('',#4806,#3875,#3876);
#3292=AXIS2_PLACEMENT_3D('',#4808,#3878,#3879);
#3293=AXIS2_PLACEMENT_3D('',#4810,#3881,#3882);
#3294=AXIS2_PLACEMENT_3D('',#4812,#3884,#3885);
#3295=AXIS2_PLACEMENT_3D('',#4813,#3886,#3887);
#3296=AXIS2_PLACEMENT_3D('',#4814,#3888,#3889);
#3297=AXIS2_PLACEMENT_3D('',#4815,#3890,#3891);
#3298=AXIS2_PLACEMENT_3D('',#4817,#3892,#3893);
#3299=AXIS2_PLACEMENT_3D('',#4820,#3895,#3896);
#3300=AXIS2_PLACEMENT_3D('',#4821,#3897,#3898);
#3301=AXIS2_PLACEMENT_3D('',#4823,#3899,#3900);
#3302=AXIS2_PLACEMENT_3D('',#4826,#3902,#3903);
#3303=AXIS2_PLACEMENT_3D('',#4827,#3904,#3905);
#3304=AXIS2_PLACEMENT_3D('',#4828,#3906,#3907);
#3305=AXIS2_PLACEMENT_3D('',#4829,#3908,#3909);
#3306=AXIS2_PLACEMENT_3D('',#4830,#3910,#3911);
#3307=AXIS2_PLACEMENT_3D('',#4832,#3912,#3913);
#3308=AXIS2_PLACEMENT_3D('',#4835,#3915,#3916);
#3309=AXIS2_PLACEMENT_3D('',#4836,#3917,#3918);
#3310=AXIS2_PLACEMENT_3D('',#4838,#3919,#3920);
#3311=AXIS2_PLACEMENT_3D('',#4841,#3922,#3923);
#3312=AXIS2_PLACEMENT_3D('',#4842,#3924,#3925);
#3313=AXIS2_PLACEMENT_3D('',#4843,#3926,#3927);
#3314=AXIS2_PLACEMENT_3D('',#4844,#3928,#3929);
#3315=AXIS2_PLACEMENT_3D('',#4845,#3930,#3931);
#3316=AXIS2_PLACEMENT_3D('',#4847,#3932,#3933);
#3317=AXIS2_PLACEMENT_3D('',#4850,#3935,#3936);
#3318=AXIS2_PLACEMENT_3D('',#4851,#3937,#3938);
#3319=AXIS2_PLACEMENT_3D('',#4852,#3939,#3940);
#3320=AXIS2_PLACEMENT_3D('',#4854,#3941,#3942);
#3321=AXIS2_PLACEMENT_3D('',#4857,#3944,#3945);
#3322=AXIS2_PLACEMENT_3D('',#4858,#3946,#3947);
#3323=AXIS2_PLACEMENT_3D('',#4859,#3948,#3949);
#3324=AXIS2_PLACEMENT_3D('',#4860,#3950,#3951);
#3325=AXIS2_PLACEMENT_3D('',#4861,#3952,#3953);
#3326=AXIS2_PLACEMENT_3D('',#4870,#3958,#3959);
#3327=AXIS2_PLACEMENT_3D('',#4876,#3963,#3964);
#3328=AXIS2_PLACEMENT_3D('',#4882,#3968,#3969);
#3329=AXIS2_PLACEMENT_3D('',#4888,#3973,#3974);
#3330=AXIS2_PLACEMENT_3D('',#4894,#3978,#3979);
#3331=AXIS2_PLACEMENT_3D('',#4897,#3982,#3983);
#3332=AXIS2_PLACEMENT_3D('',#4898,#3984,#3985);
#3333=AXIS2_PLACEMENT_3D('',#4899,#3986,#3987);
#3334=AXIS2_PLACEMENT_3D('',#4901,#3988,#3989);
#3335=AXIS2_PLACEMENT_3D('',#4902,#3990,#3991);
#3336=AXIS2_PLACEMENT_3D('',#4904,#3992,#3993);
#3337=AXIS2_PLACEMENT_3D('',#4905,#3994,#3995);
#3338=AXIS2_PLACEMENT_3D('',#4907,#3996,#3997);
#3339=AXIS2_PLACEMENT_3D('',#4909,#3999,#4000);
#3340=AXIS2_PLACEMENT_3D('',#4911,#4001,#4002);
#3341=AXIS2_PLACEMENT_3D('',#4913,#4004,#4005);
#3342=AXIS2_PLACEMENT_3D('',#4915,#4006,#4007);
#3343=AXIS2_PLACEMENT_3D('',#4917,#4009,#4010);
#3344=AXIS2_PLACEMENT_3D('',#4919,#4011,#4012);
#3345=AXIS2_PLACEMENT_3D('',#4920,#4013,#4014);
#3346=AXIS2_PLACEMENT_3D('',#4922,#4015,#4016);
#3347=AXIS2_PLACEMENT_3D('',#4924,#4018,#4019);
#3348=AXIS2_PLACEMENT_3D('',#4926,#4021,#4022);
#3349=AXIS2_PLACEMENT_3D('',#4927,#4023,#4024);
#3350=AXIS2_PLACEMENT_3D('',#4928,#4025,#4026);
#3351=AXIS2_PLACEMENT_3D('',#4930,#4027,#4028);
#3352=AXIS2_PLACEMENT_3D('',#4933,#4030,#4031);
#3353=AXIS2_PLACEMENT_3D('',#4934,#4032,#4033);
#3354=AXIS2_PLACEMENT_3D('',#4936,#4034,#4035);
#3355=AXIS2_PLACEMENT_3D('',#4939,#4037,#4038);
#3356=AXIS2_PLACEMENT_3D('',#4940,#4039,#4040);
#3357=AXIS2_PLACEMENT_3D('',#4945,#4042,#4043);
#3358=AXIS2_PLACEMENT_3D('',#4948,#4045,#4046);
#3359=AXIS2_PLACEMENT_3D('',#4949,#4047,#4048);
#3360=AXIS2_PLACEMENT_3D('',#4955,#4052,#4053);
#3361=AXIS2_PLACEMENT_3D('',#4958,#4055,#4056);
#3362=AXIS2_PLACEMENT_3D('',#4959,#4057,#4058);
#3363=AXIS2_PLACEMENT_3D('',#4963,#4061,#4062);
#3364=AXIS2_PLACEMENT_3D('',#4964,#4063,#4064);
#3365=AXIS2_PLACEMENT_3D('',#4965,#4065,#4066);
#3366=AXIS2_PLACEMENT_3D('',#4966,#4067,#4068);
#3367=AXIS2_PLACEMENT_3D('',#4967,#4069,#4070);
#3368=AXIS2_PLACEMENT_3D('',#4968,#4071,#4072);
#3369=AXIS2_PLACEMENT_3D('',#4969,#4073,#4074);
#3370=AXIS2_PLACEMENT_3D('',#4971,#4075,#4076);
#3371=AXIS2_PLACEMENT_3D('',#4974,#4078,#4079);
#3372=AXIS2_PLACEMENT_3D('',#4975,#4080,#4081);
#3373=AXIS2_PLACEMENT_3D('',#4976,#4082,#4083);
#3374=AXIS2_PLACEMENT_3D('',#4978,#4084,#4085);
#3375=AXIS2_PLACEMENT_3D('',#4981,#4087,#4088);
#3376=AXIS2_PLACEMENT_3D('',#4982,#4089,#4090);
#3377=AXIS2_PLACEMENT_3D('',#4984,#4091,#4092);
#3378=AXIS2_PLACEMENT_3D('',#4987,#4094,#4095);
#3379=AXIS2_PLACEMENT_3D('',#4988,#4096,#4097);
#3380=AXIS2_PLACEMENT_3D('',#4998,#4102,#4103);
#3381=AXIS2_PLACEMENT_3D('',#4999,#4104,#4105);
#3382=AXIS2_PLACEMENT_3D('',#5005,#4109,#4110);
#3383=AXIS2_PLACEMENT_3D('',#5009,#4113,#4114);
#3384=AXIS2_PLACEMENT_3D('',#5013,#4117,#4118);
#3385=AXIS2_PLACEMENT_3D('',#5015,#4120,#4121);
#3386=AXIS2_PLACEMENT_3D('',#5016,#4122,#4123);
#3387=AXIS2_PLACEMENT_3D('',#5018,#4124,#4125);
#3388=AXIS2_PLACEMENT_3D('',#5021,#4127,#4128);
#3389=AXIS2_PLACEMENT_3D('',#5022,#4129,#4130);
#3390=AXIS2_PLACEMENT_3D('',#5027,#4132,#4133);
#3391=AXIS2_PLACEMENT_3D('',#5030,#4135,#4136);
#3392=AXIS2_PLACEMENT_3D('',#5031,#4137,#4138);
#3393=AXIS2_PLACEMENT_3D('',#5037,#4142,#4143);
#3394=AXIS2_PLACEMENT_3D('',#5043,#4147,#4148);
#3395=AXIS2_PLACEMENT_3D('',#5049,#4152,#4153);
#3396=AXIS2_PLACEMENT_3D('',#5053,#4156,#4157);
#3397=AXIS2_PLACEMENT_3D('',#5057,#4160,#4161);
#3398=AXIS2_PLACEMENT_3D('',#5059,#4163,#4164);
#3399=AXIS2_PLACEMENT_3D('',#5060,#4165,#4166);
#3400=AXIS2_PLACEMENT_3D('',#5061,#4167,#4168);
#3401=AXIS2_PLACEMENT_3D('',#5062,#4169,#4170);
#3402=AXIS2_PLACEMENT_3D('',#5063,#4171,#4172);
#3403=AXIS2_PLACEMENT_3D('',#5065,#4174,#4175);
#3404=AXIS2_PLACEMENT_3D('',#5066,#4176,#4177);
#3405=AXIS2_PLACEMENT_3D('',#5068,#4178,#4179);
#3406=AXIS2_PLACEMENT_3D('',#5071,#4181,#4182);
#3407=AXIS2_PLACEMENT_3D('',#5072,#4183,#4184);
#3408=AXIS2_PLACEMENT_3D('',#5074,#4185,#4186);
#3409=AXIS2_PLACEMENT_3D('',#5077,#4188,#4189);
#3410=AXIS2_PLACEMENT_3D('',#5078,#4190,#4191);
#3411=AXIS2_PLACEMENT_3D('',#5079,#4192,#4193);
#3412=AXIS2_PLACEMENT_3D('',#5080,#4194,#4195);
#3413=AXIS2_PLACEMENT_3D('',#5081,#4196,#4197);
#3414=AXIS2_PLACEMENT_3D('',#5159,#4199,#4200);
#3415=AXIS2_PLACEMENT_3D('',#5161,#4201,#4202);
#3416=AXIS2_PLACEMENT_3D('',#5162,#4203,#4204);
#3417=AXIS2_PLACEMENT_3D('',#5164,#4205,#4206);
#3418=AXIS2_PLACEMENT_3D('',#5166,#4208,#4209);
#3419=AXIS2_PLACEMENT_3D('',#5168,#4210,#4211);
#3420=AXIS2_PLACEMENT_3D('',#5170,#4213,#4214);
#3421=AXIS2_PLACEMENT_3D('',#5172,#4215,#4216);
#3422=AXIS2_PLACEMENT_3D('',#5173,#4217,#4218);
#3423=AXIS2_PLACEMENT_3D('',#5175,#4219,#4220);
#3424=AXIS2_PLACEMENT_3D('',#5178,#4223,#4224);
#3425=AXIS2_PLACEMENT_3D('',#5180,#4225,#4226);
#3426=AXIS2_PLACEMENT_3D('',#5182,#4228,#4229);
#3427=AXIS2_PLACEMENT_3D('',#5183,#4230,#4231);
#3428=AXIS2_PLACEMENT_3D('',#5184,#4232,#4233);
#3429=AXIS2_PLACEMENT_3D('',#5186,#4234,#4235);
#3430=AXIS2_PLACEMENT_3D('',#5189,#4237,#4238);
#3431=AXIS2_PLACEMENT_3D('',#5190,#4239,#4240);
#3432=AXIS2_PLACEMENT_3D('',#5192,#4241,#4242);
#3433=AXIS2_PLACEMENT_3D('',#5195,#4244,#4245);
#3434=AXIS2_PLACEMENT_3D('',#5196,#4246,#4247);
#3435=AXIS2_PLACEMENT_3D('',#5197,#4248,#4249);
#3436=AXIS2_PLACEMENT_3D('',#5198,#4250,#4251);
#3437=AXIS2_PLACEMENT_3D('',#5199,#4252,#4253);
#3438=AXIS2_PLACEMENT_3D('',#5200,#4254,#4255);
#3439=AXIS2_PLACEMENT_3D('',#5201,#4256,#4257);
#3440=AXIS2_PLACEMENT_3D('',#5202,#4258,#4259);
#3441=AXIS2_PLACEMENT_3D('',#5203,#4260,#4261);
#3442=AXIS2_PLACEMENT_3D('',#5205,#4262,#4263);
#3443=AXIS2_PLACEMENT_3D('',#5206,#4264,#4265);
#3444=AXIS2_PLACEMENT_3D('',#5261,#4266,#4267);
#3445=AXIS2_PLACEMENT_3D('',#5264,#4268,#4269);
#3446=AXIS2_PLACEMENT_3D('',#5266,#4271,#4272);
#3447=AXIS2_PLACEMENT_3D('',#5272,#4276,#4277);
#3448=AXIS2_PLACEMENT_3D('',#5274,#4278,#4279);
#3449=AXIS2_PLACEMENT_3D('',#5276,#4281,#4282);
#3450=AXIS2_PLACEMENT_3D('',#5277,#4283,#4284);
#3451=AXIS2_PLACEMENT_3D('',#5278,#4285,#4286);
#3452=AXIS2_PLACEMENT_3D('',#5279,#4287,#4288);
#3453=AXIS2_PLACEMENT_3D('',#5280,#4289,#4290);
#3454=AXIS2_PLACEMENT_3D('',#5281,#4291,#4292);
#3455=AXIS2_PLACEMENT_3D('',#5282,#4293,#4294);
#3456=AXIS2_PLACEMENT_3D('',#5283,#4295,#4296);
#3457=AXIS2_PLACEMENT_3D('',#5284,#4297,#4298);
#3458=AXIS2_PLACEMENT_3D('',#5285,#4299,#4300);
#3459=AXIS2_PLACEMENT_3D('',#5286,#4301,#4302);
#3460=AXIS2_PLACEMENT_3D('',#5287,#4303,#4304);
#3461=AXIS2_PLACEMENT_3D('',#5288,#4305,#4306);
#3462=AXIS2_PLACEMENT_3D('',#5290,#4307,#4308);
#3463=AXIS2_PLACEMENT_3D('',#5294,#4310,#4311);
#3464=AXIS2_PLACEMENT_3D('',#5295,#4312,#4313);
#3465=AXIS2_PLACEMENT_3D('',#5296,#4314,#4315);
#3466=AXIS2_PLACEMENT_3D('',#5298,#4316,#4317);
#3467=AXIS2_PLACEMENT_3D('',#5300,#4318,#4319);
#3468=AXIS2_PLACEMENT_3D('',#5301,#4320,#4321);
#3469=AXIS2_PLACEMENT_3D('',#5302,#4322,#4323);
#3470=AXIS2_PLACEMENT_3D('',#5305,#4325,#4326);
#3471=AXIS2_PLACEMENT_3D('',#5306,#4327,#4328);
#3472=AXIS2_PLACEMENT_3D('',#5307,#4329,#4330);
#3473=AXIS2_PLACEMENT_3D('',#5308,#4331,#4332);
#3474=AXIS2_PLACEMENT_3D('',#5309,#4333,#4334);
#3475=AXIS2_PLACEMENT_3D('',#5311,#4335,#4336);
#3476=AXIS2_PLACEMENT_3D('',#5314,#4338,#4339);
#3477=AXIS2_PLACEMENT_3D('',#5315,#4340,#4341);
#3478=AXIS2_PLACEMENT_3D('',#5317,#4342,#4343);
#3479=AXIS2_PLACEMENT_3D('',#5320,#4345,#4346);
#3480=AXIS2_PLACEMENT_3D('',#5321,#4347,#4348);
#3481=AXIS2_PLACEMENT_3D('',#5322,#4349,#4350);
#3482=AXIS2_PLACEMENT_3D('',#5323,#4351,#4352);
#3483=AXIS2_PLACEMENT_3D('',#5324,#4353,#4354);
#3484=AXIS2_PLACEMENT_3D('',#5336,#4356,#4357);
#3485=AXIS2_PLACEMENT_3D('',#5352,#4358,#4359);
#3486=AXIS2_PLACEMENT_3D('',#5354,#4360,#4361);
#3487=AXIS2_PLACEMENT_3D('',#5380,#4363,#4364);
#3488=AXIS2_PLACEMENT_3D('',#5383,#4367,#4368);
#3489=AXIS2_PLACEMENT_3D('',#5385,#4370,#4371);
#3490=AXIS2_PLACEMENT_3D('',#5387,#4373,#4374);
#3491=AXIS2_PLACEMENT_3D('',#5389,#4375,#4376);
#3492=AXIS2_PLACEMENT_3D('',#5392,#4378,#4379);
#3493=AXIS2_PLACEMENT_3D('',#5393,#4380,#4381);
#3494=AXIS2_PLACEMENT_3D('',#5395,#4383,#4384);
#3495=AXIS2_PLACEMENT_3D('',#5397,#4386,#4387);
#3496=AXIS2_PLACEMENT_3D('',#5398,#4388,#4389);
#3497=AXIS2_PLACEMENT_3D('',#5399,#4390,#4391);
#3498=AXIS2_PLACEMENT_3D('',#5400,#4392,#4393);
#3499=AXIS2_PLACEMENT_3D('',#5401,#4394,#4395);
#3500=AXIS2_PLACEMENT_3D('',#5402,#4396,#4397);
#3501=AXIS2_PLACEMENT_3D('',#5403,#4398,#4399);
#3502=AXIS2_PLACEMENT_3D('',#5404,#4400,#4401);
#3503=AXIS2_PLACEMENT_3D('',#5405,#4402,#4403);
#3504=AXIS2_PLACEMENT_3D('',#5406,#4404,#4405);
#3505=AXIS2_PLACEMENT_3D('',#5407,#4406,#4407);
#3506=AXIS2_PLACEMENT_3D('',#5408,#4408,#4409);
#3507=AXIS2_PLACEMENT_3D('',#5409,#4410,#4411);
#3508=AXIS2_PLACEMENT_3D('',#5410,#4412,#4413);
#3509=AXIS2_PLACEMENT_3D('',#5411,#4414,#4415);
#3510=AXIS2_PLACEMENT_3D('',#5412,#4416,#4417);
#3511=DIRECTION('axis',(0.,0.,1.));
#3512=DIRECTION('refdir',(1.,0.,0.));
#3513=DIRECTION('axis',(0.,0.,1.));
#3514=DIRECTION('refdir',(1.,0.,0.));
#3515=DIRECTION('axis',(0.,0.,1.));
#3516=DIRECTION('refdir',(1.,0.,0.));
#3517=DIRECTION('center_axis',(0.,1.,0.));
#3518=DIRECTION('ref_axis',(1.,0.,0.));
#3519=DIRECTION('center_axis',(0.,-1.,0.));
#3520=DIRECTION('ref_axis',(1.,0.,0.));
#3521=DIRECTION('',(0.,-1.,0.));
#3522=DIRECTION('center_axis',(0.,-1.,0.));
#3523=DIRECTION('ref_axis',(1.,0.,0.));
#3524=DIRECTION('center_axis',(1.,0.,0.));
#3525=DIRECTION('ref_axis',(0.,0.,-1.));
#3526=DIRECTION('',(0.,-1.,0.));
#3527=DIRECTION('',(0.,0.,-1.));
#3528=DIRECTION('',(0.,1.,0.));
#3529=DIRECTION('',(0.,0.,1.));
#3530=DIRECTION('center_axis',(-1.,0.,0.));
#3531=DIRECTION('ref_axis',(0.,0.,1.));
#3532=DIRECTION('',(0.,1.,0.));
#3533=DIRECTION('',(0.,0.,-1.));
#3534=DIRECTION('',(0.,1.,0.));
#3535=DIRECTION('',(0.,0.,1.));
#3536=DIRECTION('center_axis',(0.,1.,0.));
#3537=DIRECTION('ref_axis',(1.,0.,0.));
#3538=DIRECTION('center_axis',(0.,1.,0.));
#3539=DIRECTION('ref_axis',(1.,0.,0.));
#3540=DIRECTION('',(-1.,0.,0.));
#3541=DIRECTION('center_axis',(0.,1.,0.));
#3542=DIRECTION('ref_axis',(1.,0.,0.));
#3543=DIRECTION('center_axis',(0.,1.,0.));
#3544=DIRECTION('ref_axis',(1.,0.,0.));
#3545=DIRECTION('center_axis',(0.,1.,0.));
#3546=DIRECTION('ref_axis',(1.,0.,0.));
#3547=DIRECTION('',(1.,0.,0.));
#3548=DIRECTION('center_axis',(0.,0.,1.));
#3549=DIRECTION('ref_axis',(1.,0.,0.));
#3550=DIRECTION('center_axis',(0.,0.,1.));
#3551=DIRECTION('ref_axis',(1.,0.,0.));
#3552=DIRECTION('',(0.,0.,1.));
#3553=DIRECTION('center_axis',(0.,0.,-1.));
#3554=DIRECTION('ref_axis',(1.,0.,0.));
#3555=DIRECTION('center_axis',(0.,0.,1.));
#3556=DIRECTION('ref_axis',(1.,0.,0.));
#3557=DIRECTION('center_axis',(0.,0.,1.));
#3558=DIRECTION('ref_axis',(1.,0.,0.));
#3559=DIRECTION('',(0.,0.,1.));
#3560=DIRECTION('center_axis',(0.,0.,-1.));
#3561=DIRECTION('ref_axis',(1.,0.,0.));
#3562=DIRECTION('center_axis',(1.,0.,0.));
#3563=DIRECTION('ref_axis',(0.,0.,-1.));
#3564=DIRECTION('center_axis',(1.,0.,0.));
#3565=DIRECTION('ref_axis',(0.,0.,-1.));
#3566=DIRECTION('',(1.,0.,0.));
#3567=DIRECTION('center_axis',(-1.,0.,0.));
#3568=DIRECTION('ref_axis',(0.,0.,-1.));
#3569=DIRECTION('center_axis',(0.,1.,0.));
#3570=DIRECTION('ref_axis',(1.,0.,0.));
#3571=DIRECTION('',(-1.,0.,0.));
#3572=DIRECTION('',(0.,0.,1.));
#3573=DIRECTION('',(-1.,0.,0.));
#3574=DIRECTION('',(0.,0.,-1.));
#3575=DIRECTION('center_axis',(1.,0.,0.));
#3576=DIRECTION('ref_axis',(0.,0.,-1.));
#3577=DIRECTION('',(0.,-1.,0.));
#3578=DIRECTION('',(0.,0.,-1.));
#3579=DIRECTION('',(0.,1.,0.));
#3580=DIRECTION('center_axis',(-1.,0.,0.));
#3581=DIRECTION('ref_axis',(0.,0.,1.));
#3582=DIRECTION('',(0.,1.,0.));
#3583=DIRECTION('',(0.,1.,0.));
#3584=DIRECTION('',(0.,0.,1.));
#3585=DIRECTION('center_axis',(0.,0.,1.));
#3586=DIRECTION('ref_axis',(1.,0.,0.));
#3587=DIRECTION('',(1.,0.,0.));
#3588=DIRECTION('center_axis',(0.,1.,0.));
#3589=DIRECTION('ref_axis',(0.,0.,1.));
#3590=DIRECTION('',(1.,0.,0.));
#3591=DIRECTION('center_axis',(0.,1.,0.));
#3592=DIRECTION('ref_axis',(1.,0.,0.));
#3593=DIRECTION('center_axis',(0.,1.,0.));
#3594=DIRECTION('ref_axis',(1.,0.,0.));
#3595=DIRECTION('',(0.,1.,0.));
#3596=DIRECTION('center_axis',(0.,-1.,0.));
#3597=DIRECTION('ref_axis',(1.,0.,0.));
#3598=DIRECTION('center_axis',(0.,1.,0.));
#3599=DIRECTION('ref_axis',(1.,0.,0.));
#3600=DIRECTION('',(-1.,0.,0.));
#3601=DIRECTION('',(0.,0.,1.));
#3602=DIRECTION('',(-1.,0.,0.));
#3603=DIRECTION('',(0.,0.,-1.));
#3604=DIRECTION('center_axis',(1.,0.,0.));
#3605=DIRECTION('ref_axis',(0.,0.,-1.));
#3606=DIRECTION('',(0.,-1.,0.));
#3607=DIRECTION('',(0.,0.,-1.));
#3608=DIRECTION('',(0.,1.,0.));
#3609=DIRECTION('center_axis',(-1.,0.,0.));
#3610=DIRECTION('ref_axis',(0.,0.,1.));
#3611=DIRECTION('',(0.,1.,0.));
#3612=DIRECTION('',(0.,1.,0.));
#3613=DIRECTION('',(0.,0.,1.));
#3614=DIRECTION('center_axis',(0.,0.,1.));
#3615=DIRECTION('ref_axis',(1.,0.,0.));
#3616=DIRECTION('',(1.,0.,0.));
#3617=DIRECTION('center_axis',(0.,1.,0.));
#3618=DIRECTION('ref_axis',(0.,0.,1.));
#3619=DIRECTION('',(1.,0.,0.));
#3620=DIRECTION('center_axis',(0.,1.,0.));
#3621=DIRECTION('ref_axis',(1.,0.,0.));
#3622=DIRECTION('',(-1.,0.,0.));
#3623=DIRECTION('',(0.,0.,1.));
#3624=DIRECTION('',(-1.,0.,0.));
#3625=DIRECTION('',(0.,0.,-1.));
#3626=DIRECTION('center_axis',(1.,0.,0.));
#3627=DIRECTION('ref_axis',(0.,0.,-1.));
#3628=DIRECTION('',(0.,-1.,0.));
#3629=DIRECTION('',(0.,0.,-1.));
#3630=DIRECTION('',(0.,1.,0.));
#3631=DIRECTION('center_axis',(-1.,0.,0.));
#3632=DIRECTION('ref_axis',(0.,0.,1.));
#3633=DIRECTION('',(0.,1.,0.));
#3634=DIRECTION('',(0.,1.,0.));
#3635=DIRECTION('',(0.,0.,1.));
#3636=DIRECTION('center_axis',(0.,0.,1.));
#3637=DIRECTION('ref_axis',(1.,0.,0.));
#3638=DIRECTION('',(1.,0.,0.));
#3639=DIRECTION('center_axis',(0.,1.,0.));
#3640=DIRECTION('ref_axis',(0.,0.,1.));
#3641=DIRECTION('',(1.,0.,0.));
#3642=DIRECTION('center_axis',(0.,1.,0.));
#3643=DIRECTION('ref_axis',(-1.,0.,0.));
#3644=DIRECTION('',(-1.,0.,0.));
#3645=DIRECTION('',(0.,0.,1.));
#3646=DIRECTION('',(-1.,0.,0.));
#3647=DIRECTION('',(0.,0.,1.));
#3648=DIRECTION('center_axis',(1.,0.,0.));
#3649=DIRECTION('ref_axis',(0.,1.,0.));
#3650=DIRECTION('',(0.,1.,0.));
#3651=DIRECTION('',(0.,1.,0.));
#3652=DIRECTION('',(0.,0.,1.));
#3653=DIRECTION('center_axis',(0.,-1.,0.));
#3654=DIRECTION('ref_axis',(1.,0.,0.));
#3655=DIRECTION('',(1.,0.,0.));
#3656=DIRECTION('',(1.,0.,0.));
#3657=DIRECTION('',(0.,0.,1.));
#3658=DIRECTION('center_axis',(-1.,0.,0.));
#3659=DIRECTION('ref_axis',(0.,-1.,0.));
#3660=DIRECTION('',(0.,-1.,0.));
#3661=DIRECTION('',(0.,-1.,0.));
#3662=DIRECTION('center_axis',(0.,0.,1.));
#3663=DIRECTION('ref_axis',(1.,0.,0.));
#3664=DIRECTION('center_axis',(0.,0.,1.));
#3665=DIRECTION('ref_axis',(1.,0.,0.));
#3666=DIRECTION('axis',(0.,0.,1.));
#3667=DIRECTION('refdir',(1.,0.,0.));
#3668=DIRECTION('center_axis',(0.,1.,0.));
#3669=DIRECTION('ref_axis',(0.,0.,1.));
#3670=DIRECTION('center_axis',(0.,1.,0.));
#3671=DIRECTION('ref_axis',(1.,0.,0.));
#3672=DIRECTION('center_axis',(0.,-1.,0.));
#3673=DIRECTION('ref_axis',(1.,0.,0.));
#3674=DIRECTION('',(0.,1.,0.));
#3675=DIRECTION('center_axis',(0.,-1.,0.));
#3676=DIRECTION('ref_axis',(1.,0.,0.));
#3677=DIRECTION('center_axis',(0.,-1.,0.));
#3678=DIRECTION('ref_axis',(1.,0.,0.));
#3679=DIRECTION('center_axis',(0.,1.,0.));
#3680=DIRECTION('ref_axis',(1.,0.,0.));
#3681=DIRECTION('',(-0.866025403784439,-0.5,-1.06057523872491E-16));
#3682=DIRECTION('center_axis',(1.92296268638356E-16,0.,-1.));
#3683=DIRECTION('ref_axis',(-1.,0.,-1.92296268638356E-16));
#3684=DIRECTION('',(0.,1.,0.));
#3685=DIRECTION('',(-1.,0.,-1.92296268638356E-16));
#3686=DIRECTION('',(0.,1.,0.));
#3687=DIRECTION('center_axis',(0.866025403784439,0.,-0.5));
#3688=DIRECTION('ref_axis',(-0.5,0.,-0.866025403784439));
#3689=DIRECTION('',(0.,1.,0.));
#3690=DIRECTION('',(-0.5,0.,-0.866025403784439));
#3691=DIRECTION('center_axis',(0.866025403784439,0.,0.5));
#3692=DIRECTION('ref_axis',(0.5,0.,-0.866025403784439));
#3693=DIRECTION('',(0.,1.,0.));
#3694=DIRECTION('',(0.5,0.,-0.866025403784439));
#3695=DIRECTION('center_axis',(-1.92296268638356E-16,0.,1.));
#3696=DIRECTION('ref_axis',(1.,0.,1.92296268638356E-16));
#3697=DIRECTION('',(0.,1.,0.));
#3698=DIRECTION('',(1.,0.,1.92296268638356E-16));
#3699=DIRECTION('center_axis',(-0.866025403784439,0.,0.5));
#3700=DIRECTION('ref_axis',(0.5,0.,0.866025403784439));
#3701=DIRECTION('',(0.,1.,0.));
#3702=DIRECTION('',(0.5,0.,0.866025403784439));
#3703=DIRECTION('center_axis',(-0.866025403784439,0.,-0.5));
#3704=DIRECTION('ref_axis',(-0.5,0.,0.866025403784439));
#3705=DIRECTION('',(-0.5,0.,0.866025403784438));
#3706=DIRECTION('center_axis',(0.,1.,0.));
#3707=DIRECTION('ref_axis',(0.,0.,1.));
#3708=DIRECTION('center_axis',(0.,1.,0.));
#3709=DIRECTION('ref_axis',(1.,0.,0.));
#3710=DIRECTION('axis',(0.,0.,1.));
#3711=DIRECTION('refdir',(1.,0.,0.));
#3712=DIRECTION('center_axis',(0.,0.,1.));
#3713=DIRECTION('ref_axis',(1.,0.,0.));
#3714=DIRECTION('center_axis',(0.,0.,1.));
#3715=DIRECTION('ref_axis',(1.,0.,0.));
#3716=DIRECTION('',(0.,0.,1.));
#3717=DIRECTION('center_axis',(0.,0.,-1.));
#3718=DIRECTION('ref_axis',(1.,0.,0.));
#3719=DIRECTION('center_axis',(0.,0.,1.));
#3720=DIRECTION('ref_axis',(1.,0.,0.));
#3721=DIRECTION('center_axis',(0.,0.,1.));
#3722=DIRECTION('ref_axis',(1.,0.,0.));
#3723=DIRECTION('',(0.,0.,1.));
#3724=DIRECTION('center_axis',(0.,0.,-1.));
#3725=DIRECTION('ref_axis',(1.,0.,0.));
#3726=DIRECTION('center_axis',(0.,1.,0.));
#3727=DIRECTION('ref_axis',(1.,0.,0.));
#3728=DIRECTION('center_axis',(0.,1.,0.));
#3729=DIRECTION('ref_axis',(1.,0.,0.));
#3730=DIRECTION('',(0.,0.,-1.));
#3731=DIRECTION('',(-1.,0.,0.));
#3732=DIRECTION('',(0.,0.,1.));
#3733=DIRECTION('',(-1.,0.,0.));
#3734=DIRECTION('center_axis',(0.,1.,0.));
#3735=DIRECTION('ref_axis',(1.,0.,0.));
#3736=DIRECTION('',(0.,1.,0.));
#3737=DIRECTION('',(0.,-1.,0.));
#3738=DIRECTION('center_axis',(0.,1.,0.));
#3739=DIRECTION('ref_axis',(1.,0.,0.));
#3740=DIRECTION('',(0.,-1.,0.));
#3741=DIRECTION('center_axis',(0.,1.,0.));
#3742=DIRECTION('ref_axis',(1.,0.,0.));
#3743=DIRECTION('',(0.,-1.,0.));
#3744=DIRECTION('center_axis',(0.,-1.,0.));
#3745=DIRECTION('ref_axis',(1.,0.,0.));
#3746=DIRECTION('',(0.,1.,0.));
#3747=DIRECTION('center_axis',(0.,1.,0.));
#3748=DIRECTION('ref_axis',(1.,0.,0.));
#3749=DIRECTION('center_axis',(0.,1.,0.));
#3750=DIRECTION('ref_axis',(1.,0.,0.));
#3751=DIRECTION('center_axis',(0.,1.,0.));
#3752=DIRECTION('ref_axis',(0.,0.,1.));
#3753=DIRECTION('',(1.,0.,0.));
#3754=DIRECTION('',(0.,0.,-1.));
#3755=DIRECTION('',(1.,0.,0.));
#3756=DIRECTION('',(0.,0.,1.));
#3757=DIRECTION('center_axis',(0.,0.,1.));
#3758=DIRECTION('ref_axis',(1.,0.,0.));
#3759=DIRECTION('',(0.,1.,0.));
#3760=DIRECTION('center_axis',(1.,0.,0.));
#3761=DIRECTION('ref_axis',(0.,0.,-1.));
#3762=DIRECTION('',(0.,-1.,0.));
#3763=DIRECTION('center_axis',(-1.,0.,0.));
#3764=DIRECTION('ref_axis',(0.,0.,1.));
#3765=DIRECTION('',(0.,1.,0.));
#3766=DIRECTION('center_axis',(0.,1.,0.));
#3767=DIRECTION('ref_axis',(0.,0.,1.));
#3768=DIRECTION('',(1.,0.,0.));
#3769=DIRECTION('',(0.,0.,-1.));
#3770=DIRECTION('',(1.,0.,0.));
#3771=DIRECTION('',(0.,0.,1.));
#3772=DIRECTION('center_axis',(0.,0.,1.));
#3773=DIRECTION('ref_axis',(1.,0.,0.));
#3774=DIRECTION('',(-1.,0.,0.));
#3775=DIRECTION('',(0.,1.,0.));
#3776=DIRECTION('center_axis',(0.,1.,0.));
#3777=DIRECTION('ref_axis',(1.,0.,0.));
#3778=DIRECTION('',(0.,0.,-1.));
#3779=DIRECTION('',(-1.,0.,0.));
#3780=DIRECTION('',(0.,0.,1.));
#3781=DIRECTION('center_axis',(1.,0.,0.));
#3782=DIRECTION('ref_axis',(0.,0.,-1.));
#3783=DIRECTION('',(0.,-1.,0.));
#3784=DIRECTION('center_axis',(-1.,0.,0.));
#3785=DIRECTION('ref_axis',(0.,0.,1.));
#3786=DIRECTION('',(0.,1.,0.));
#3787=DIRECTION('center_axis',(0.,1.,0.));
#3788=DIRECTION('ref_axis',(-1.,0.,0.));
#3789=DIRECTION('',(-1.,0.,0.));
#3790=DIRECTION('',(0.,0.,1.));
#3791=DIRECTION('',(-1.,0.,0.));
#3792=DIRECTION('',(0.,0.,1.));
#3793=DIRECTION('center_axis',(1.,0.,0.));
#3794=DIRECTION('ref_axis',(0.,1.,0.));
#3795=DIRECTION('',(0.,1.,0.));
#3796=DIRECTION('',(0.,1.,0.));
#3797=DIRECTION('',(0.,0.,1.));
#3798=DIRECTION('center_axis',(0.,-1.,0.));
#3799=DIRECTION('ref_axis',(1.,0.,0.));
#3800=DIRECTION('',(1.,0.,0.));
#3801=DIRECTION('',(1.,0.,0.));
#3802=DIRECTION('',(0.,0.,1.));
#3803=DIRECTION('center_axis',(-1.,0.,0.));
#3804=DIRECTION('ref_axis',(0.,-1.,0.));
#3805=DIRECTION('',(0.,-1.,0.));
#3806=DIRECTION('',(0.,-1.,0.));
#3807=DIRECTION('center_axis',(0.,0.,1.));
#3808=DIRECTION('ref_axis',(1.,0.,0.));
#3809=DIRECTION('center_axis',(0.,0.,1.));
#3810=DIRECTION('ref_axis',(1.,0.,0.));
#3811=DIRECTION('axis',(0.,0.,1.));
#3812=DIRECTION('refdir',(1.,0.,0.));
#3813=DIRECTION('axis',(0.,0.,1.));
#3814=DIRECTION('refdir',(1.,0.,0.));
#3815=DIRECTION('center_axis',(0.,1.,0.));
#3816=DIRECTION('ref_axis',(1.,0.,0.));
#3817=DIRECTION('center_axis',(0.,1.,0.));
#3818=DIRECTION('ref_axis',(1.,0.,0.));
#3819=DIRECTION('',(0.,1.,0.));
#3820=DIRECTION('center_axis',(0.,-1.,0.));
#3821=DIRECTION('ref_axis',(1.,0.,0.));
#3822=DIRECTION('center_axis',(0.,1.,0.));
#3823=DIRECTION('ref_axis',(1.,0.,0.));
#3824=DIRECTION('center_axis',(0.,1.,0.));
#3825=DIRECTION('ref_axis',(1.,0.,0.));
#3826=DIRECTION('',(0.,1.,0.));
#3827=DIRECTION('center_axis',(0.,-1.,0.));
#3828=DIRECTION('ref_axis',(1.,0.,0.));
#3829=DIRECTION('center_axis',(0.,1.,0.));
#3830=DIRECTION('ref_axis',(1.,0.,0.));
#3831=DIRECTION('center_axis',(0.,1.,0.));
#3832=DIRECTION('ref_axis',(1.,0.,0.));
#3833=DIRECTION('',(0.,1.,0.));
#3834=DIRECTION('center_axis',(0.,-1.,0.));
#3835=DIRECTION('ref_axis',(1.,0.,0.));
#3836=DIRECTION('center_axis',(0.,1.,0.));
#3837=DIRECTION('ref_axis',(-0.996194698091745,0.,-0.0871557427476579));
#3838=DIRECTION('',(0.,-1.,0.));
#3839=DIRECTION('center_axis',(0.,1.,0.));
#3840=DIRECTION('ref_axis',(1.,0.,0.));
#3841=DIRECTION('',(0.,1.,0.));
#3842=DIRECTION('center_axis',(0.,1.,0.));
#3843=DIRECTION('ref_axis',(1.,0.,0.));
#3844=DIRECTION('center_axis',(0.,1.,0.));
#3845=DIRECTION('ref_axis',(1.,0.,0.));
#3846=DIRECTION('',(-0.996194698091746,0.,-0.0871557427476579));
#3847=DIRECTION('center_axis',(0.,1.,0.));
#3848=DIRECTION('ref_axis',(1.,0.,0.));
#3849=DIRECTION('',(-0.996194698091746,0.,-0.0871557427476579));
#3850=DIRECTION('center_axis',(0.,1.,0.));
#3851=DIRECTION('ref_axis',(1.,0.,0.));
#3852=DIRECTION('',(0.996194698091746,0.,0.087155742747658));
#3853=DIRECTION('center_axis',(0.,1.,0.));
#3854=DIRECTION('ref_axis',(1.,0.,0.));
#3855=DIRECTION('',(0.996194698091746,0.,0.087155742747658));
#3856=DIRECTION('center_axis',(0.0871557427476579,0.,-0.996194698091746));
#3857=DIRECTION('ref_axis',(-0.996194698091746,0.,-0.0871557427476579));
#3858=DIRECTION('',(-0.996194698091746,0.,-0.0871557427476579));
#3859=DIRECTION('',(0.,-1.,0.));
#3860=DIRECTION('center_axis',(0.,1.,0.));
#3861=DIRECTION('ref_axis',(1.,0.,0.));
#3862=DIRECTION('center_axis',(0.,1.,0.));
#3863=DIRECTION('ref_axis',(1.,0.,0.));
#3864=DIRECTION('',(0.,1.,0.));
#3865=DIRECTION('center_axis',(0.,1.,0.));
#3866=DIRECTION('ref_axis',(1.,0.,0.));
#3867=DIRECTION('',(0.,1.,0.));
#3868=DIRECTION('',(0.,-1.,0.));
#3869=DIRECTION('center_axis',(0.,1.,0.));
#3870=DIRECTION('ref_axis',(1.,0.,0.));
#3871=DIRECTION('center_axis',(0.,1.,0.));
#3872=DIRECTION('ref_axis',(1.,0.,0.));
#3873=DIRECTION('',(0.996194698091746,0.,0.087155742747658));
#3874=DIRECTION('',(0.996194698091746,0.,0.087155742747658));
#3875=DIRECTION('center_axis',(0.,1.,0.));
#3876=DIRECTION('ref_axis',(1.,0.,0.));
#3877=DIRECTION('',(-0.996194698091746,0.,-0.0871557427476579));
#3878=DIRECTION('center_axis',(-0.087155742747658,0.,0.996194698091746));
#3879=DIRECTION('ref_axis',(0.996194698091746,0.,0.087155742747658));
#3880=DIRECTION('',(0.,-1.,0.));
#3881=DIRECTION('center_axis',(0.0871557427476579,0.,-0.996194698091746));
#3882=DIRECTION('ref_axis',(-0.996194698091746,0.,-0.0871557427476579));
#3883=DIRECTION('',(0.,1.,0.));
#3884=DIRECTION('center_axis',(-0.087155742747658,0.,0.996194698091746));
#3885=DIRECTION('ref_axis',(0.996194698091746,0.,0.087155742747658));
#3886=DIRECTION('center_axis',(0.,1.,0.));
#3887=DIRECTION('ref_axis',(1.,0.,0.));
#3888=DIRECTION('axis',(0.,0.,1.));
#3889=DIRECTION('refdir',(1.,0.,0.));
#3890=DIRECTION('center_axis',(0.,1.,0.));
#3891=DIRECTION('ref_axis',(1.,0.,0.));
#3892=DIRECTION('center_axis',(0.,-1.,0.));
#3893=DIRECTION('ref_axis',(1.,0.,0.));
#3894=DIRECTION('',(0.,-1.,0.));
#3895=DIRECTION('center_axis',(0.,-1.,0.));
#3896=DIRECTION('ref_axis',(1.,0.,0.));
#3897=DIRECTION('center_axis',(0.,1.,0.));
#3898=DIRECTION('ref_axis',(1.,0.,0.));
#3899=DIRECTION('center_axis',(0.,1.,0.));
#3900=DIRECTION('ref_axis',(1.,0.,0.));
#3901=DIRECTION('',(0.,-1.,0.));
#3902=DIRECTION('center_axis',(0.,1.,0.));
#3903=DIRECTION('ref_axis',(1.,0.,0.));
#3904=DIRECTION('center_axis',(0.,1.,0.));
#3905=DIRECTION('ref_axis',(1.,0.,0.));
#3906=DIRECTION('center_axis',(0.,1.,0.));
#3907=DIRECTION('ref_axis',(1.,0.,0.));
#3908=DIRECTION('axis',(0.,0.,1.));
#3909=DIRECTION('refdir',(1.,0.,0.));
#3910=DIRECTION('center_axis',(0.,1.,0.));
#3911=DIRECTION('ref_axis',(1.,0.,0.));
#3912=DIRECTION('center_axis',(0.,-1.,0.));
#3913=DIRECTION('ref_axis',(1.,0.,0.));
#3914=DIRECTION('',(0.,-1.,0.));
#3915=DIRECTION('center_axis',(0.,-1.,0.));
#3916=DIRECTION('ref_axis',(1.,0.,0.));
#3917=DIRECTION('center_axis',(0.,1.,0.));
#3918=DIRECTION('ref_axis',(1.,0.,0.));
#3919=DIRECTION('center_axis',(0.,1.,0.));
#3920=DIRECTION('ref_axis',(1.,0.,0.));
#3921=DIRECTION('',(0.,-1.,0.));
#3922=DIRECTION('center_axis',(0.,1.,0.));
#3923=DIRECTION('ref_axis',(1.,0.,0.));
#3924=DIRECTION('center_axis',(0.,1.,0.));
#3925=DIRECTION('ref_axis',(1.,0.,0.));
#3926=DIRECTION('center_axis',(0.,1.,0.));
#3927=DIRECTION('ref_axis',(1.,0.,0.));
#3928=DIRECTION('axis',(0.,0.,1.));
#3929=DIRECTION('refdir',(1.,0.,0.));
#3930=DIRECTION('center_axis',(0.,1.,0.));
#3931=DIRECTION('ref_axis',(1.,0.,0.));
#3932=DIRECTION('center_axis',(0.,1.,0.));
#3933=DIRECTION('ref_axis',(1.,0.,0.));
#3934=DIRECTION('',(0.,1.,0.));
#3935=DIRECTION('center_axis',(0.,-1.,0.));
#3936=DIRECTION('ref_axis',(1.,0.,0.));
#3937=DIRECTION('center_axis',(0.,1.,0.));
#3938=DIRECTION('ref_axis',(1.,0.,0.));
#3939=DIRECTION('center_axis',(0.,1.,0.));
#3940=DIRECTION('ref_axis',(1.,0.,0.));
#3941=DIRECTION('center_axis',(0.,1.,0.));
#3942=DIRECTION('ref_axis',(1.,0.,0.));
#3943=DIRECTION('',(0.,-1.,0.));
#3944=DIRECTION('center_axis',(0.,1.,0.));
#3945=DIRECTION('ref_axis',(1.,0.,0.));
#3946=DIRECTION('center_axis',(0.,1.,0.));
#3947=DIRECTION('ref_axis',(1.,0.,0.));
#3948=DIRECTION('center_axis',(0.,1.,0.));
#3949=DIRECTION('ref_axis',(1.,0.,0.));
#3950=DIRECTION('axis',(0.,0.,1.));
#3951=DIRECTION('refdir',(1.,0.,0.));
#3952=DIRECTION('center_axis',(0.866025403784439,0.,-0.5));
#3953=DIRECTION('ref_axis',(0.5,0.,0.866025403784439));
#3954=DIRECTION('',(-0.5,0.,-0.866025403784439));
#3955=DIRECTION('',(0.,-1.,0.));
#3956=DIRECTION('',(0.5,0.,0.866025403784439));
#3957=DIRECTION('',(0.,-1.,0.));
#3958=DIRECTION('center_axis',(1.20185167898973E-16,0.,-1.));
#3959=DIRECTION('ref_axis',(1.,0.,1.20185167898973E-16));
#3960=DIRECTION('',(-1.,0.,-1.20185167898973E-16));
#3961=DIRECTION('',(0.,-1.,0.));
#3962=DIRECTION('',(1.,0.,1.20185167898973E-16));
#3963=DIRECTION('center_axis',(-0.866025403784439,0.,-0.5));
#3964=DIRECTION('ref_axis',(0.5,0.,-0.866025403784439));
#3965=DIRECTION('',(-0.5,0.,0.866025403784439));
#3966=DIRECTION('',(0.,-1.,0.));
#3967=DIRECTION('',(0.5,0.,-0.866025403784439));
#3968=DIRECTION('center_axis',(-0.866025403784439,0.,0.5));
#3969=DIRECTION('ref_axis',(-0.5,0.,-0.866025403784439));
#3970=DIRECTION('',(0.5,0.,0.866025403784439));
#3971=DIRECTION('',(0.,-1.,0.));
#3972=DIRECTION('',(-0.5,0.,-0.866025403784439));
#3973=DIRECTION('center_axis',(-2.40370335797945E-16,0.,1.));
#3974=DIRECTION('ref_axis',(-1.,0.,-2.40370335797945E-16));
#3975=DIRECTION('',(1.,0.,2.40370335797945E-16));
#3976=DIRECTION('',(0.,-1.,0.));
#3977=DIRECTION('',(-1.,0.,-2.40370335797945E-16));
#3978=DIRECTION('center_axis',(0.866025403784439,0.,0.5));
#3979=DIRECTION('ref_axis',(-0.5,0.,0.866025403784439));
#3980=DIRECTION('',(0.5,0.,-0.866025403784439));
#3981=DIRECTION('',(-0.5,0.,0.866025403784439));
#3982=DIRECTION('center_axis',(0.,1.,0.));
#3983=DIRECTION('ref_axis',(1.,0.,0.));
#3984=DIRECTION('center_axis',(0.,-1.,0.));
#3985=DIRECTION('ref_axis',(0.,0.,-1.));
#3986=DIRECTION('center_axis',(0.,1.,0.));
#3987=DIRECTION('ref_axis',(1.,0.,0.));
#3988=DIRECTION('center_axis',(0.,1.,0.));
#3989=DIRECTION('ref_axis',(1.,0.,0.));
#3990=DIRECTION('center_axis',(0.,1.,0.));
#3991=DIRECTION('ref_axis',(0.,0.,1.));
#3992=DIRECTION('center_axis',(0.,-1.,0.));
#3993=DIRECTION('ref_axis',(1.,0.,0.));
#3994=DIRECTION('center_axis',(0.,-1.,0.));
#3995=DIRECTION('ref_axis',(1.,0.,0.));
#3996=DIRECTION('center_axis',(0.,-1.,0.));
#3997=DIRECTION('ref_axis',(1.,0.,0.));
#3998=DIRECTION('',(0.707106781186548,0.707106781186547,8.65956056235493E-17));
#3999=DIRECTION('center_axis',(0.,-1.,0.));
#4000=DIRECTION('ref_axis',(1.,0.,0.));
#4001=DIRECTION('center_axis',(0.,-1.,0.));
#4002=DIRECTION('ref_axis',(1.,0.,0.));
#4003=DIRECTION('',(0.,1.,0.));
#4004=DIRECTION('center_axis',(0.,1.,0.));
#4005=DIRECTION('ref_axis',(1.,0.,0.));
#4006=DIRECTION('center_axis',(0.,-1.,0.));
#4007=DIRECTION('ref_axis',(1.,0.,0.));
#4008=DIRECTION('',(-0.707106781186547,0.707106781186548,-8.65956056235493E-17));
#4009=DIRECTION('center_axis',(0.,-1.,0.));
#4010=DIRECTION('ref_axis',(0.,0.,-1.));
#4011=DIRECTION('center_axis',(0.,-1.,0.));
#4012=DIRECTION('ref_axis',(1.,0.,0.));
#4013=DIRECTION('center_axis',(0.,1.,0.));
#4014=DIRECTION('ref_axis',(1.,0.,0.));
#4015=DIRECTION('center_axis',(0.,1.,0.));
#4016=DIRECTION('ref_axis',(1.,0.,0.));
#4017=DIRECTION('',(-0.447213595499958,0.894427190999916,-5.47678698264203E-17));
#4018=DIRECTION('center_axis',(0.,-1.,0.));
#4019=DIRECTION('ref_axis',(1.,0.,0.));
#4020=DIRECTION('',(0.,1.,0.));
#4021=DIRECTION('axis',(0.,0.,1.));
#4022=DIRECTION('refdir',(1.,0.,0.));
#4023=DIRECTION('axis',(0.,0.,1.));
#4024=DIRECTION('refdir',(1.,0.,0.));
#4025=DIRECTION('center_axis',(0.,1.,0.));
#4026=DIRECTION('ref_axis',(1.,0.,0.));
#4027=DIRECTION('center_axis',(0.,1.,0.));
#4028=DIRECTION('ref_axis',(1.,0.,0.));
#4029=DIRECTION('',(0.,1.,0.));
#4030=DIRECTION('center_axis',(0.,-1.,0.));
#4031=DIRECTION('ref_axis',(1.,0.,0.));
#4032=DIRECTION('center_axis',(0.,1.,0.));
#4033=DIRECTION('ref_axis',(1.,0.,0.));
#4034=DIRECTION('center_axis',(0.,1.,0.));
#4035=DIRECTION('ref_axis',(1.,0.,0.));
#4036=DIRECTION('',(0.,1.,0.));
#4037=DIRECTION('center_axis',(0.,-1.,0.));
#4038=DIRECTION('ref_axis',(1.,0.,0.));
#4039=DIRECTION('center_axis',(0.,1.,0.));
#4040=DIRECTION('ref_axis',(1.,0.,0.));
#4041=DIRECTION('',(0.,-1.,0.));
#4042=DIRECTION('center_axis',(0.,1.,0.));
#4043=DIRECTION('ref_axis',(1.,0.,0.));
#4044=DIRECTION('',(0.,1.,0.));
#4045=DIRECTION('center_axis',(0.,1.,0.));
#4046=DIRECTION('ref_axis',(1.,0.,0.));
#4047=DIRECTION('center_axis',(0.0484198570820323,0.,-0.998827070838669));
#4048=DIRECTION('ref_axis',(-0.998827070838669,0.,-0.0484198570820323));
#4049=DIRECTION('',(-0.998827070838669,0.,-0.0484198570820323));
#4050=DIRECTION('',(0.,-1.,0.));
#4051=DIRECTION('',(-0.998827070838669,0.,-0.0484198570820323));
#4052=DIRECTION('center_axis',(0.,1.,0.));
#4053=DIRECTION('ref_axis',(1.,0.,0.));
#4054=DIRECTION('',(0.998827070838669,0.,0.0484198570820322));
#4055=DIRECTION('center_axis',(0.,1.,0.));
#4056=DIRECTION('ref_axis',(1.,0.,0.));
#4057=DIRECTION('center_axis',(-0.0484198570820322,0.,0.998827070838669));
#4058=DIRECTION('ref_axis',(0.998827070838669,0.,0.0484198570820322));
#4059=DIRECTION('',(0.998827070838669,0.,0.0484198570820322));
#4060=DIRECTION('',(0.,1.,0.));
#4061=DIRECTION('center_axis',(0.,1.,0.));
#4062=DIRECTION('ref_axis',(-0.998827070838669,0.,-0.0484198570820321));
#4063=DIRECTION('center_axis',(0.,1.,0.));
#4064=DIRECTION('ref_axis',(1.,0.,0.));
#4065=DIRECTION('center_axis',(0.,1.,0.));
#4066=DIRECTION('ref_axis',(1.,0.,0.));
#4067=DIRECTION('',(0.,0.,1.));
#4068=DIRECTION('',(1.,0.,0.));
#4069=DIRECTION('axis',(0.,0.,1.));
#4070=DIRECTION('refdir',(1.,0.,0.));
#4071=DIRECTION('axis',(0.,0.,1.));
#4072=DIRECTION('refdir',(1.,0.,0.));
#4073=DIRECTION('center_axis',(1.,0.,0.));
#4074=DIRECTION('ref_axis',(0.,0.,-1.));
#4075=DIRECTION('center_axis',(1.,0.,0.));
#4076=DIRECTION('ref_axis',(0.,0.,-1.));
#4077=DIRECTION('',(1.,0.,0.));
#4078=DIRECTION('center_axis',(-1.,0.,0.));
#4079=DIRECTION('ref_axis',(0.,0.,-1.));
#4080=DIRECTION('center_axis',(1.,0.,0.));
#4081=DIRECTION('ref_axis',(0.,0.,-1.));
#4082=DIRECTION('center_axis',(1.,0.,0.));
#4083=DIRECTION('ref_axis',(0.,0.,-1.));
#4084=DIRECTION('center_axis',(1.,0.,0.));
#4085=DIRECTION('ref_axis',(0.,0.,-1.));
#4086=DIRECTION('',(1.,0.,0.));
#4087=DIRECTION('center_axis',(-1.,0.,0.));
#4088=DIRECTION('ref_axis',(0.,0.,-1.));
#4089=DIRECTION('center_axis',(1.,0.,0.));
#4090=DIRECTION('ref_axis',(0.,0.,-1.));
#4091=DIRECTION('center_axis',(1.,0.,0.));
#4092=DIRECTION('ref_axis',(0.,0.,-1.));
#4093=DIRECTION('',(1.,0.,0.));
#4094=DIRECTION('center_axis',(-1.,0.,0.));
#4095=DIRECTION('ref_axis',(0.,0.,-1.));
#4096=DIRECTION('center_axis',(1.,0.,0.));
#4097=DIRECTION('ref_axis',(0.,0.,-1.));
#4098=DIRECTION('',(0.,0.,-1.));
#4099=DIRECTION('',(0.,-1.,0.));
#4100=DIRECTION('',(0.,0.,1.));
#4101=DIRECTION('',(0.,1.,0.));
#4102=DIRECTION('center_axis',(1.,0.,0.));
#4103=DIRECTION('ref_axis',(0.,0.,-1.));
#4104=DIRECTION('center_axis',(0.,0.,1.));
#4105=DIRECTION('ref_axis',(0.,-1.,0.));
#4106=DIRECTION('',(1.,0.,0.));
#4107=DIRECTION('',(0.,-1.,0.));
#4108=DIRECTION('',(1.,0.,0.));
#4109=DIRECTION('center_axis',(0.,1.,0.));
#4110=DIRECTION('ref_axis',(0.,0.,1.));
#4111=DIRECTION('',(0.,0.,1.));
#4112=DIRECTION('',(1.,0.,0.));
#4113=DIRECTION('center_axis',(0.,0.,-1.));
#4114=DIRECTION('ref_axis',(0.,1.,0.));
#4115=DIRECTION('',(0.,1.,0.));
#4116=DIRECTION('',(1.,0.,0.));
#4117=DIRECTION('center_axis',(0.,-1.,0.));
#4118=DIRECTION('ref_axis',(0.,0.,-1.));
#4119=DIRECTION('',(0.,0.,-1.));
#4120=DIRECTION('center_axis',(1.,0.,0.));
#4121=DIRECTION('ref_axis',(0.,0.,-1.));
#4122=DIRECTION('center_axis',(0.,1.,0.));
#4123=DIRECTION('ref_axis',(1.,0.,0.));
#4124=DIRECTION('center_axis',(0.,1.,0.));
#4125=DIRECTION('ref_axis',(1.,0.,0.));
#4126=DIRECTION('',(0.,1.,0.));
#4127=DIRECTION('center_axis',(0.,-1.,0.));
#4128=DIRECTION('ref_axis',(1.,0.,0.));
#4129=DIRECTION('center_axis',(0.,1.,0.));
#4130=DIRECTION('ref_axis',(-1.,0.,1.22464679914735E-16));
#4131=DIRECTION('',(0.,1.,0.));
#4132=DIRECTION('center_axis',(0.,1.,0.));
#4133=DIRECTION('ref_axis',(1.,0.,0.));
#4134=DIRECTION('',(0.,1.,0.));
#4135=DIRECTION('center_axis',(0.,1.,0.));
#4136=DIRECTION('ref_axis',(1.,0.,0.));
#4137=DIRECTION('center_axis',(0.,1.,0.));
#4138=DIRECTION('ref_axis',(1.,0.,0.));
#4139=DIRECTION('',(1.,0.,0.));
#4140=DIRECTION('',(0.,0.,1.));
#4141=DIRECTION('',(-1.,0.,0.));
#4142=DIRECTION('center_axis',(-1.,0.,0.));
#4143=DIRECTION('ref_axis',(0.,0.,1.));
#4144=DIRECTION('',(0.,1.,0.));
#4145=DIRECTION('',(0.,0.,-1.));
#4146=DIRECTION('',(0.,1.,0.));
#4147=DIRECTION('center_axis',(0.,1.,0.));
#4148=DIRECTION('ref_axis',(1.,0.,0.));
#4149=DIRECTION('',(-1.,0.,0.));
#4150=DIRECTION('',(1.,0.,0.));
#4151=DIRECTION('',(0.,0.,-1.));
#4152=DIRECTION('center_axis',(0.,0.,-1.));
#4153=DIRECTION('ref_axis',(-1.,0.,0.));
#4154=DIRECTION('',(-1.,0.,0.));
#4155=DIRECTION('',(0.,1.,0.));
#4156=DIRECTION('center_axis',(0.,0.,1.));
#4157=DIRECTION('ref_axis',(1.,0.,0.));
#4158=DIRECTION('',(1.,0.,0.));
#4159=DIRECTION('',(0.,1.,0.));
#4160=DIRECTION('center_axis',(1.,0.,0.));
#4161=DIRECTION('ref_axis',(0.,0.,-1.));
#4162=DIRECTION('',(0.,0.,-1.));
#4163=DIRECTION('center_axis',(1.,0.,0.));
#4164=DIRECTION('ref_axis',(0.,0.,-1.));
#4165=DIRECTION('center_axis',(0.,1.,0.));
#4166=DIRECTION('ref_axis',(0.,0.,1.));
#4167=DIRECTION('center_axis',(1.,0.,0.));
#4168=DIRECTION('ref_axis',(0.,0.,-1.));
#4169=DIRECTION('center_axis',(1.,0.,0.));
#4170=DIRECTION('ref_axis',(0.,0.,-1.));
#4171=DIRECTION('center_axis',(1.,0.,0.));
#4172=DIRECTION('ref_axis',(0.,0.,-1.));
#4173=DIRECTION('',(-1.,0.,0.));
#4174=DIRECTION('axis',(0.,0.,1.));
#4175=DIRECTION('refdir',(1.,0.,0.));
#4176=DIRECTION('center_axis',(0.,1.,0.));
#4177=DIRECTION('ref_axis',(1.,0.,0.));
#4178=DIRECTION('center_axis',(0.,-1.,0.));
#4179=DIRECTION('ref_axis',(1.,0.,0.));
#4180=DIRECTION('',(0.,-1.,0.));
#4181=DIRECTION('center_axis',(0.,-1.,0.));
#4182=DIRECTION('ref_axis',(1.,0.,0.));
#4183=DIRECTION('center_axis',(0.,1.,0.));
#4184=DIRECTION('ref_axis',(1.,0.,0.));
#4185=DIRECTION('center_axis',(0.,1.,0.));
#4186=DIRECTION('ref_axis',(1.,0.,0.));
#4187=DIRECTION('',(0.,-1.,0.));
#4188=DIRECTION('center_axis',(0.,1.,0.));
#4189=DIRECTION('ref_axis',(1.,0.,0.));
#4190=DIRECTION('center_axis',(0.,1.,0.));
#4191=DIRECTION('ref_axis',(1.,0.,0.));
#4192=DIRECTION('center_axis',(0.,1.,0.));
#4193=DIRECTION('ref_axis',(1.,0.,0.));
#4194=DIRECTION('axis',(0.,0.,1.));
#4195=DIRECTION('refdir',(1.,0.,0.));
#4196=DIRECTION('center_axis',(1.,0.,0.));
#4197=DIRECTION('ref_axis',(0.,0.,-1.));
#4198=DIRECTION('',(1.,0.,0.));
#4199=DIRECTION('center_axis',(0.,1.,0.));
#4200=DIRECTION('ref_axis',(0.,0.,1.));
#4201=DIRECTION('center_axis',(0.,-1.,0.));
#4202=DIRECTION('ref_axis',(1.,0.,0.));
#4203=DIRECTION('center_axis',(0.,-1.,0.));
#4204=DIRECTION('ref_axis',(1.,0.,0.));
#4205=DIRECTION('center_axis',(0.,-1.,0.));
#4206=DIRECTION('ref_axis',(1.,0.,0.));
#4207=DIRECTION('',(0.707106781186547,0.707106781186548,8.65956056235493E-17));
#4208=DIRECTION('center_axis',(0.,-1.,0.));
#4209=DIRECTION('ref_axis',(1.,0.,0.));
#4210=DIRECTION('center_axis',(0.,-1.,0.));
#4211=DIRECTION('ref_axis',(1.,0.,0.));
#4212=DIRECTION('',(0.,1.,0.));
#4213=DIRECTION('center_axis',(0.,-1.,0.));
#4214=DIRECTION('ref_axis',(0.,0.,-1.));
#4215=DIRECTION('center_axis',(0.,-1.,0.));
#4216=DIRECTION('ref_axis',(1.,0.,0.));
#4217=DIRECTION('center_axis',(0.,-1.,0.));
#4218=DIRECTION('ref_axis',(1.,0.,0.));
#4219=DIRECTION('center_axis',(0.,-1.,0.));
#4220=DIRECTION('ref_axis',(1.,0.,0.));
#4221=DIRECTION('',(0.,1.,0.));
#4222=DIRECTION('',(0.,1.,0.));
#4223=DIRECTION('center_axis',(0.,1.,0.));
#4224=DIRECTION('ref_axis',(1.,0.,0.));
#4225=DIRECTION('center_axis',(0.,-1.,0.));
#4226=DIRECTION('ref_axis',(1.,0.,0.));
#4227=DIRECTION('',(-0.707106781186548,0.707106781186547,-8.65956056235494E-17));
#4228=DIRECTION('center_axis',(0.,-1.,0.));
#4229=DIRECTION('ref_axis',(0.,0.,-1.));
#4230=DIRECTION('axis',(0.,0.,1.));
#4231=DIRECTION('refdir',(1.,0.,0.));
#4232=DIRECTION('center_axis',(0.,1.,0.));
#4233=DIRECTION('ref_axis',(1.,0.,0.));
#4234=DIRECTION('center_axis',(0.,-1.,0.));
#4235=DIRECTION('ref_axis',(1.,0.,0.));
#4236=DIRECTION('',(0.,-1.,0.));
#4237=DIRECTION('center_axis',(0.,-1.,0.));
#4238=DIRECTION('ref_axis',(1.,0.,0.));
#4239=DIRECTION('center_axis',(0.,1.,0.));
#4240=DIRECTION('ref_axis',(1.,0.,0.));
#4241=DIRECTION('center_axis',(0.,1.,0.));
#4242=DIRECTION('ref_axis',(1.,0.,0.));
#4243=DIRECTION('',(0.,-1.,0.));
#4244=DIRECTION('center_axis',(0.,1.,0.));
#4245=DIRECTION('ref_axis',(1.,0.,0.));
#4246=DIRECTION('center_axis',(0.,1.,0.));
#4247=DIRECTION('ref_axis',(1.,0.,0.));
#4248=DIRECTION('center_axis',(0.,1.,0.));
#4249=DIRECTION('ref_axis',(1.,0.,0.));
#4250=DIRECTION('',(0.,0.,1.));
#4251=DIRECTION('',(1.,0.,0.));
#4252=DIRECTION('',(0.,0.,1.));
#4253=DIRECTION('',(-1.,1.22464679914735E-16,0.));
#4254=DIRECTION('',(0.,0.,1.));
#4255=DIRECTION('',(1.,0.,0.));
#4256=DIRECTION('',(0.,0.,1.));
#4257=DIRECTION('',(1.,0.,0.));
#4258=DIRECTION('axis',(0.,0.,1.));
#4259=DIRECTION('refdir',(1.,0.,0.));
#4260=DIRECTION('center_axis',(-1.,0.,0.));
#4261=DIRECTION('ref_axis',(0.,0.,1.));
#4262=DIRECTION('center_axis',(0.,-1.,1.38777878078145E-16));
#4263=DIRECTION('ref_axis',(0.,-1.38777878078145E-16,-1.));
#4264=DIRECTION('center_axis',(1.,0.,0.));
#4265=DIRECTION('ref_axis',(0.,0.,1.));
#4266=DIRECTION('center_axis',(0.,1.,0.));
#4267=DIRECTION('ref_axis',(1.,0.,0.));
#4268=DIRECTION('center_axis',(0.,-1.,0.));
#4269=DIRECTION('ref_axis',(1.,0.,0.));
#4270=DIRECTION('',(0.,0.,1.));
#4271=DIRECTION('center_axis',(1.,0.,0.));
#4272=DIRECTION('ref_axis',(0.,0.,1.));
#4273=DIRECTION('',(0.,-1.,0.));
#4274=DIRECTION('',(0.,0.,1.));
#4275=DIRECTION('',(0.,-1.,0.));
#4276=DIRECTION('center_axis',(0.,-1.,0.));
#4277=DIRECTION('ref_axis',(1.,0.,0.));
#4278=DIRECTION('center_axis',(0.,-1.,0.));
#4279=DIRECTION('ref_axis',(1.,0.,0.));
#4280=DIRECTION('',(0.,1.,0.));
#4281=DIRECTION('center_axis',(0.,-1.,0.));
#4282=DIRECTION('ref_axis',(1.,0.,0.));
#4283=DIRECTION('center_axis',(0.,1.,0.));
#4284=DIRECTION('ref_axis',(1.,0.,0.));
#4285=DIRECTION('',(0.,0.,1.));
#4286=DIRECTION('',(1.,0.,0.));
#4287=DIRECTION('',(0.,0.,1.));
#4288=DIRECTION('',(1.,0.,0.));
#4289=DIRECTION('',(0.,0.,1.));
#4290=DIRECTION('',(1.,0.,0.));
#4291=DIRECTION('',(0.,0.,1.));
#4292=DIRECTION('',(1.,0.,0.));
#4293=DIRECTION('',(0.,0.,1.));
#4294=DIRECTION('',(1.,0.,0.));
#4295=DIRECTION('',(0.,0.,1.));
#4296=DIRECTION('',(1.,0.,0.));
#4297=DIRECTION('',(0.,0.,1.));
#4298=DIRECTION('',(1.,0.,0.));
#4299=DIRECTION('',(0.,0.,1.));
#4300=DIRECTION('',(1.,0.,0.));
#4301=DIRECTION('',(0.,0.,1.));
#4302=DIRECTION('',(2.22044604925031E-16,1.,0.));
#4303=DIRECTION('axis',(0.,0.,1.));
#4304=DIRECTION('refdir',(1.,0.,0.));
#4305=DIRECTION('center_axis',(-1.,0.,0.));
#4306=DIRECTION('ref_axis',(0.,1.,0.));
#4307=DIRECTION('center_axis',(-1.,0.,1.22464679914735E-16));
#4308=DIRECTION('ref_axis',(0.,1.,0.));
#4309=DIRECTION('',(1.,0.,0.));
#4310=DIRECTION('center_axis',(-1.,0.,1.22464679914735E-16));
#4311=DIRECTION('ref_axis',(0.,1.,0.));
#4312=DIRECTION('center_axis',(-1.,0.,1.22464679914735E-16));
#4313=DIRECTION('ref_axis',(0.,1.,0.));
#4314=DIRECTION('center_axis',(0.,-1.,0.));
#4315=DIRECTION('ref_axis',(0.,0.,-1.));
#4316=DIRECTION('center_axis',(0.,1.,0.));
#4317=DIRECTION('ref_axis',(0.,0.,-1.));
#4318=DIRECTION('center_axis',(1.,0.,0.));
#4319=DIRECTION('ref_axis',(0.,1.,0.));
#4320=DIRECTION('center_axis',(1.,0.,0.));
#4321=DIRECTION('ref_axis',(0.,1.,0.));
#4322=DIRECTION('center_axis',(1.,0.,0.));
#4323=DIRECTION('ref_axis',(0.,1.,0.));
#4324=DIRECTION('',(-1.,0.,0.));
#4325=DIRECTION('center_axis',(1.,0.,0.));
#4326=DIRECTION('ref_axis',(0.,1.,0.));
#4327=DIRECTION('center_axis',(-1.,0.,1.22464679914735E-16));
#4328=DIRECTION('ref_axis',(0.,1.,0.));
#4329=DIRECTION('center_axis',(1.,0.,0.));
#4330=DIRECTION('ref_axis',(0.,1.,0.));
#4331=DIRECTION('axis',(0.,0.,1.));
#4332=DIRECTION('refdir',(1.,0.,0.));
#4333=DIRECTION('center_axis',(0.,1.,0.));
#4334=DIRECTION('ref_axis',(1.,0.,0.));
#4335=DIRECTION('center_axis',(0.,-1.,0.));
#4336=DIRECTION('ref_axis',(1.,0.,0.));
#4337=DIRECTION('',(0.,-1.,0.));
#4338=DIRECTION('center_axis',(0.,-1.,0.));
#4339=DIRECTION('ref_axis',(1.,0.,0.));
#4340=DIRECTION('center_axis',(0.,1.,0.));
#4341=DIRECTION('ref_axis',(1.,0.,0.));
#4342=DIRECTION('center_axis',(0.,1.,0.));
#4343=DIRECTION('ref_axis',(1.,0.,0.));
#4344=DIRECTION('',(0.,-1.,0.));
#4345=DIRECTION('center_axis',(0.,1.,0.));
#4346=DIRECTION('ref_axis',(1.,0.,0.));
#4347=DIRECTION('center_axis',(0.,1.,0.));
#4348=DIRECTION('ref_axis',(1.,0.,0.));
#4349=DIRECTION('center_axis',(0.,1.,0.));
#4350=DIRECTION('ref_axis',(1.,0.,0.));
#4351=DIRECTION('axis',(0.,0.,1.));
#4352=DIRECTION('refdir',(1.,0.,0.));
#4353=DIRECTION('center_axis',(0.,1.,0.));
#4354=DIRECTION('ref_axis',(1.,0.,0.));
#4355=DIRECTION('',(0.866025403784439,-0.5,1.06057523872491E-16));
#4356=DIRECTION('center_axis',(0.,-1.,0.));
#4357=DIRECTION('ref_axis',(1.,0.,0.));
#4358=DIRECTION('center_axis',(0.,-1.,0.));
#4359=DIRECTION('ref_axis',(1.,0.,0.));
#4360=DIRECTION('center_axis',(0.,1.,0.));
#4361=DIRECTION('ref_axis',(1.,0.,0.));
#4362=DIRECTION('',(-0.866025403784439,-0.5,-1.06057523872491E-16));
#4363=DIRECTION('center_axis',(1.4792020664489E-16,0.,-1.));
#4364=DIRECTION('ref_axis',(-1.,0.,-1.4792020664489E-16));
#4365=DIRECTION('',(0.,1.,0.));
#4366=DIRECTION('',(0.,1.,0.));
#4367=DIRECTION('center_axis',(-0.866025403784439,0.,-0.5));
#4368=DIRECTION('ref_axis',(-0.5,0.,0.866025403784439));
#4369=DIRECTION('',(0.,1.,0.));
#4370=DIRECTION('center_axis',(-0.866025403784439,0.,0.5));
#4371=DIRECTION('ref_axis',(0.5,0.,0.866025403784439));
#4372=DIRECTION('',(0.,1.,0.));
#4373=DIRECTION('center_axis',(0.,1.,0.));
#4374=DIRECTION('ref_axis',(1.,0.,0.));
#4375=DIRECTION('center_axis',(0.,1.,0.));
#4376=DIRECTION('ref_axis',(1.,0.,0.));
#4377=DIRECTION('',(0.,-1.,0.));
#4378=DIRECTION('center_axis',(0.,1.,0.));
#4379=DIRECTION('ref_axis',(1.,0.,0.));
#4380=DIRECTION('center_axis',(-2.95840413289779E-16,0.,1.));
#4381=DIRECTION('ref_axis',(1.,0.,2.95840413289779E-16));
#4382=DIRECTION('',(0.,1.,0.));
#4383=DIRECTION('center_axis',(0.866025403784439,0.,-0.5));
#4384=DIRECTION('ref_axis',(-0.5,0.,-0.866025403784439));
#4385=DIRECTION('',(0.,1.,0.));
#4386=DIRECTION('center_axis',(0.866025403784439,0.,0.5));
#4387=DIRECTION('ref_axis',(0.5,0.,-0.866025403784439));
#4388=DIRECTION('center_axis',(0.,1.,0.));
#4389=DIRECTION('ref_axis',(1.,0.,0.));
#4390=DIRECTION('center_axis',(0.,1.,0.));
#4391=DIRECTION('ref_axis',(1.,0.,0.));
#4392=DIRECTION('',(0.,0.,1.));
#4393=DIRECTION('',(1.,0.,0.));
#4394=DIRECTION('',(0.,0.,1.));
#4395=DIRECTION('',(1.,0.,0.));
#4396=DIRECTION('',(0.,0.,1.));
#4397=DIRECTION('',(1.,0.,0.));
#4398=DIRECTION('',(0.,0.,1.));
#4399=DIRECTION('',(1.,0.,0.));
#4400=DIRECTION('',(0.,0.,1.));
#4401=DIRECTION('',(1.,0.,0.));
#4402=DIRECTION('',(0.,0.,1.));
#4403=DIRECTION('',(2.22044604925031E-16,1.,0.));
#4404=DIRECTION('',(0.,0.,1.));
#4405=DIRECTION('',(1.,0.,0.));
#4406=DIRECTION('',(0.,0.,1.));
#4407=DIRECTION('',(2.22044604925031E-16,-1.,0.));
#4408=DIRECTION('',(0.,0.,1.));
#4409=DIRECTION('',(2.22044604925031E-16,-1.,0.));
#4410=DIRECTION('',(0.,0.,1.));
#4411=DIRECTION('',(1.,0.,0.));
#4412=DIRECTION('',(0.,0.,1.));
#4413=DIRECTION('',(1.,0.,0.));
#4414=DIRECTION('',(0.,0.,1.));
#4415=DIRECTION('',(1.,0.,0.));
#4416=DIRECTION('',(0.,0.,1.));
#4417=DIRECTION('',(1.,0.,0.));
#4418=CARTESIAN_POINT('',(0.,0.,0.));
#4419=CARTESIAN_POINT('',(0.,0.,0.));
#4420=CARTESIAN_POINT('',(0.,0.,0.));
#4421=CARTESIAN_POINT('Origin',(0.,0.5,2.5));
#4422=CARTESIAN_POINT('',(-0.25,0.9,2.5));
#4423=CARTESIAN_POINT('Origin',(0.,0.9,2.5));
#4424=CARTESIAN_POINT('',(-0.25,0.5,2.5));
#4425=CARTESIAN_POINT('',(-0.25,0.5,2.5));
#4426=CARTESIAN_POINT('Origin',(0.,0.5,2.5));
#4427=CARTESIAN_POINT('Origin',(-4.18287614141286,-0.3,1.39779915763554));
#4428=CARTESIAN_POINT('',(-4.18287614141286,0.3,0.6));
#4429=CARTESIAN_POINT('',(-4.18287614141286,-0.3,0.6));
#4430=CARTESIAN_POINT('',(-4.18287614141286,-0.15,0.6));
#4431=CARTESIAN_POINT('',(-4.18287614141286,0.3,1.39779915763554));
#4432=CARTESIAN_POINT('',(-4.18287614141286,0.3,0.5));
#4433=CARTESIAN_POINT('',(-4.18287614141286,-0.3,1.39779915763554));
#4434=CARTESIAN_POINT('',(-4.18287614141286,-0.3,1.39779915763554));
#4435=CARTESIAN_POINT('',(-4.18287614141286,-0.3,0.5));
#4436=CARTESIAN_POINT('Origin',(-4.78287614141285,-0.3,0.5));
#4437=CARTESIAN_POINT('',(-4.78287614141285,-0.3,0.6));
#4438=CARTESIAN_POINT('',(-4.78287614141285,0.3,0.6));
#4439=CARTESIAN_POINT('',(-4.78287614141285,-0.15,0.6));
#4440=CARTESIAN_POINT('',(-4.78287614141285,-0.3,1.39779915763554));
#4441=CARTESIAN_POINT('',(-4.78287614141285,-0.3,1.39779915763554));
#4442=CARTESIAN_POINT('',(-4.78287614141285,0.3,1.39779915763554));
#4443=CARTESIAN_POINT('',(-4.78287614141285,-0.3,1.39779915763554));
#4444=CARTESIAN_POINT('',(-4.78287614141285,0.3,1.39779915763554));
#4445=CARTESIAN_POINT('Origin',(-4.48287614141285,-0.3,1.39779915763554));
#4446=CARTESIAN_POINT('Origin',(-4.48287614141285,-0.3,1.39779915763554));
#4447=CARTESIAN_POINT('',(-1.24143807070643,-0.3,0.6));
#4448=CARTESIAN_POINT('Origin',(-4.48287614141285,-0.3,1.39779915763554));
#4449=CARTESIAN_POINT('Origin',(-4.48287614141285,0.3,1.39779915763554));
#4450=CARTESIAN_POINT('Origin',(-4.48287614141285,0.3,1.39779915763554));
#4451=CARTESIAN_POINT('',(-1.24143807070643,0.3,0.6));
#4452=CARTESIAN_POINT('Origin',(-6.8,0.,-0.1));
#4453=CARTESIAN_POINT('',(-7.075,-3.36777869765523E-17,0.));
#4454=CARTESIAN_POINT('Origin',(-6.8,0.,0.));
#4455=CARTESIAN_POINT('',(-7.075,3.36777869765523E-17,0.6));
#4456=CARTESIAN_POINT('',(-7.075,-3.36777869765523E-17,-0.1));
#4457=CARTESIAN_POINT('Origin',(-6.8,0.,0.6));
#4458=CARTESIAN_POINT('Origin',(10.8,0.,-0.1));
#4459=CARTESIAN_POINT('',(10.525,-3.36777869765523E-17,0.));
#4460=CARTESIAN_POINT('Origin',(10.8,0.,0.));
#4461=CARTESIAN_POINT('',(10.525,3.36777869765523E-17,0.6));
#4462=CARTESIAN_POINT('',(10.525,-3.36777869765523E-17,-0.1));
#4463=CARTESIAN_POINT('Origin',(10.8,0.,0.6));
#4464=CARTESIAN_POINT('Origin',(6.4,0.,2.5));
#4465=CARTESIAN_POINT('',(6.5,-7.47034547479885E-17,3.11));
#4466=CARTESIAN_POINT('Origin',(6.5,0.,2.5));
#4467=CARTESIAN_POINT('',(8.5,7.47034547479885E-17,3.11));
#4468=CARTESIAN_POINT('',(6.4,-7.47034547479885E-17,3.11));
#4469=CARTESIAN_POINT('Origin',(8.5,0.,2.5));
#4470=CARTESIAN_POINT('Origin',(7.5,-0.9,2.));
#4471=CARTESIAN_POINT('',(8.5,-0.9,0.6));
#4472=CARTESIAN_POINT('',(6.5,-0.9,0.6));
#4473=CARTESIAN_POINT('',(4.75,-0.9,0.6));
#4474=CARTESIAN_POINT('',(8.5,-0.9,3.5));
#4475=CARTESIAN_POINT('',(8.5,-0.9,0.5));
#4476=CARTESIAN_POINT('',(6.5,-0.9,3.5));
#4477=CARTESIAN_POINT('',(8.5,-0.9,3.5));
#4478=CARTESIAN_POINT('',(6.5,-0.9,3.5));
#4479=CARTESIAN_POINT('Origin',(8.5,-0.9,3.5));
#4480=CARTESIAN_POINT('',(8.5,0.9,0.6));
#4481=CARTESIAN_POINT('',(8.5,-0.45,0.6));
#4482=CARTESIAN_POINT('',(8.5,0.9,3.5));
#4483=CARTESIAN_POINT('',(8.5,0.9,0.5));
#4484=CARTESIAN_POINT('',(8.5,-0.9,3.5));
#4485=CARTESIAN_POINT('Origin',(6.5,-0.9,0.5));
#4486=CARTESIAN_POINT('',(6.5,0.9,0.6));
#4487=CARTESIAN_POINT('',(6.5,-0.45,0.6));
#4488=CARTESIAN_POINT('',(6.5,0.9,3.5));
#4489=CARTESIAN_POINT('',(6.5,-0.9,3.5));
#4490=CARTESIAN_POINT('',(6.5,0.9,3.5));
#4491=CARTESIAN_POINT('Origin',(6.5,-0.9,3.5));
#4492=CARTESIAN_POINT('',(8.5,0.9,3.5));
#4493=CARTESIAN_POINT('Origin',(7.5,0.9,2.));
#4494=CARTESIAN_POINT('',(4.75,0.9,0.6));
#4495=CARTESIAN_POINT('Origin',(0.,-1.,2.5));
#4496=CARTESIAN_POINT('',(-0.31,-0.9,2.5));
#4497=CARTESIAN_POINT('Origin',(0.,-0.9,2.5));
#4498=CARTESIAN_POINT('',(-0.31,-0.5,2.5));
#4499=CARTESIAN_POINT('',(-0.31,-1.,2.5));
#4500=CARTESIAN_POINT('Origin',(0.,-0.5,2.5));
#4501=CARTESIAN_POINT('Origin',(0.,0.5,1.9));
#4502=CARTESIAN_POINT('',(0.7,0.5,0.6));
#4503=CARTESIAN_POINT('',(-0.7,0.5,0.6));
#4504=CARTESIAN_POINT('',(1.,0.5,0.6));
#4505=CARTESIAN_POINT('',(0.7,0.5,3.3));
#4506=CARTESIAN_POINT('',(0.7,0.5,0.5));
#4507=CARTESIAN_POINT('',(-0.7,0.5,3.3));
#4508=CARTESIAN_POINT('',(0.7,0.5,3.3));
#4509=CARTESIAN_POINT('',(-0.7,0.5,3.3));
#4510=CARTESIAN_POINT('Origin',(0.7,0.5,3.3));
#4511=CARTESIAN_POINT('',(0.7,0.9,0.6));
#4512=CARTESIAN_POINT('',(0.7,0.25,0.6));
#4513=CARTESIAN_POINT('',(0.7,0.9,3.3));
#4514=CARTESIAN_POINT('',(0.7,0.9,0.5));
#4515=CARTESIAN_POINT('',(0.7,0.5,3.3));
#4516=CARTESIAN_POINT('Origin',(-0.7,0.5,0.5));
#4517=CARTESIAN_POINT('',(-0.7,0.9,0.6));
#4518=CARTESIAN_POINT('',(-0.7,0.25,0.6));
#4519=CARTESIAN_POINT('',(-0.7,0.9,3.3));
#4520=CARTESIAN_POINT('',(-0.7,0.5,3.3));
#4521=CARTESIAN_POINT('',(-0.7,0.9,3.3));
#4522=CARTESIAN_POINT('Origin',(-0.7,0.5,3.3));
#4523=CARTESIAN_POINT('',(0.7,0.9,3.3));
#4524=CARTESIAN_POINT('Origin',(0.,0.9,1.9));
#4525=CARTESIAN_POINT('',(1.,0.9,0.6));
#4526=CARTESIAN_POINT('Origin',(0.,-0.9,1.9));
#4527=CARTESIAN_POINT('',(0.7,-0.9,0.6));
#4528=CARTESIAN_POINT('',(-0.7,-0.9,0.6));
#4529=CARTESIAN_POINT('',(1.,-0.9,0.6));
#4530=CARTESIAN_POINT('',(0.7,-0.9,3.3));
#4531=CARTESIAN_POINT('',(0.7,-0.9,0.5));
#4532=CARTESIAN_POINT('',(-0.7,-0.9,3.3));
#4533=CARTESIAN_POINT('',(0.7,-0.9,3.3));
#4534=CARTESIAN_POINT('',(-0.7,-0.9,3.3));
#4535=CARTESIAN_POINT('Origin',(0.7,-0.9,3.3));
#4536=CARTESIAN_POINT('',(0.7,-0.5,0.6));
#4537=CARTESIAN_POINT('',(0.7,-0.45,0.6));
#4538=CARTESIAN_POINT('',(0.7,-0.5,3.3));
#4539=CARTESIAN_POINT('',(0.7,-0.5,0.5));
#4540=CARTESIAN_POINT('',(0.7,-0.9,3.3));
#4541=CARTESIAN_POINT('Origin',(-0.7,-0.9,0.5));
#4542=CARTESIAN_POINT('',(-0.7,-0.5,0.6));
#4543=CARTESIAN_POINT('',(-0.7,-0.45,0.6));
#4544=CARTESIAN_POINT('',(-0.7,-0.5,3.3));
#4545=CARTESIAN_POINT('',(-0.7,-0.9,3.3));
#4546=CARTESIAN_POINT('',(-0.7,-0.5,3.3));
#4547=CARTESIAN_POINT('Origin',(-0.7,-0.9,3.3));
#4548=CARTESIAN_POINT('',(0.7,-0.5,3.3));
#4549=CARTESIAN_POINT('Origin',(0.,-0.5,1.9));
#4550=CARTESIAN_POINT('',(1.,-0.5,0.6));
#4551=CARTESIAN_POINT('Origin',(11.5,1.25,0.));
#4552=CARTESIAN_POINT('',(11.5,1.25,0.));
#4553=CARTESIAN_POINT('',(-7.5,1.25,0.));
#4554=CARTESIAN_POINT('',(11.5,1.25,0.));
#4555=CARTESIAN_POINT('',(-7.5,1.25,0.6));
#4556=CARTESIAN_POINT('',(-7.5,1.25,0.));
#4557=CARTESIAN_POINT('',(11.5,1.25,0.6));
#4558=CARTESIAN_POINT('',(11.5,1.25,0.6));
#4559=CARTESIAN_POINT('',(11.5,1.25,0.));
#4560=CARTESIAN_POINT('Origin',(11.5,-1.25,0.));
#4561=CARTESIAN_POINT('',(11.5,-1.25,0.));
#4562=CARTESIAN_POINT('',(11.5,-1.25,0.));
#4563=CARTESIAN_POINT('',(11.5,-1.25,0.6));
#4564=CARTESIAN_POINT('',(11.5,-1.25,0.6));
#4565=CARTESIAN_POINT('',(11.5,-1.25,0.));
#4566=CARTESIAN_POINT('Origin',(-7.5,-1.25,0.));
#4567=CARTESIAN_POINT('',(-7.5,-1.25,0.));
#4568=CARTESIAN_POINT('',(-7.5,-1.25,0.));
#4569=CARTESIAN_POINT('',(-7.5,-1.25,0.6));
#4570=CARTESIAN_POINT('',(-7.5,-1.25,0.6));
#4571=CARTESIAN_POINT('',(-7.5,-1.25,0.));
#4572=CARTESIAN_POINT('Origin',(-7.5,1.25,0.));
#4573=CARTESIAN_POINT('',(-7.5,1.25,0.));
#4574=CARTESIAN_POINT('',(-7.5,1.25,0.6));
#4575=CARTESIAN_POINT('Origin',(2.,0.,0.6));
#4576=CARTESIAN_POINT('Origin',(2.,0.,0.));
#4577=CARTESIAN_POINT('',(0.,0.,0.));
#4578=CARTESIAN_POINT('Origin',(0.,-2.,0.));
#4579=CARTESIAN_POINT('',(-0.2942,-2.,3.60291088309151E-17));
#4580=CARTESIAN_POINT('Origin',(0.,-2.,0.));
#4581=CARTESIAN_POINT('Origin',(0.,-1.445,0.));
#4582=CARTESIAN_POINT('',(-0.2942,0.,-3.60291088309151E-17));
#4583=CARTESIAN_POINT('',(-0.2942,-1.445,-3.60291088309151E-17));
#4584=CARTESIAN_POINT('Origin',(0.,0.,0.));
#4585=CARTESIAN_POINT('Origin',(0.,0.341586508806388,0.));
#4586=CARTESIAN_POINT('',(-0.475,0.4,-5.81707229594993E-17));
#4587=CARTESIAN_POINT('Origin',(0.,0.4,0.));
#4588=CARTESIAN_POINT('',(-0.577350269189626,0.340908044531739,-7.07050159149938E-17));
#4589=CARTESIAN_POINT('',(-0.576175134594813,0.341586508806388,-7.05611034329833E-17));
#4590=CARTESIAN_POINT('',(-0.288675134594813,0.340908044531739,0.5));
#4591=CARTESIAN_POINT('Ctrl Pts',(-0.288675134594813,0.340908044531739,
0.5));
#4592=CARTESIAN_POINT('Ctrl Pts',(-0.433012701893303,0.424241377863696,
0.249999999998124));
#4593=CARTESIAN_POINT('Ctrl Pts',(-0.577350269189626,0.340908044531739,
-7.07050159149938E-17));
#4594=CARTESIAN_POINT('',(0.288675134594813,0.340908044531739,0.5));
#4595=CARTESIAN_POINT('Ctrl Pts',(0.288675134594813,0.340908044531739,0.5));
#4596=CARTESIAN_POINT('Ctrl Pts',(-2.16648921025353E-12,0.424241377863696,
0.5));
#4597=CARTESIAN_POINT('Ctrl Pts',(-0.288675134594813,0.340908044531739,
0.5));
#4598=CARTESIAN_POINT('',(0.577350269189626,0.340908044531739,0.));
#4599=CARTESIAN_POINT('Ctrl Pts',(0.577350269189626,0.340908044531739,0.));
#4600=CARTESIAN_POINT('Ctrl Pts',(0.433012701891136,0.424241377863697,0.250000000001876));
#4601=CARTESIAN_POINT('Ctrl Pts',(0.288675134594813,0.340908044531739,0.5));
#4602=CARTESIAN_POINT('',(0.288675134594813,0.340908044531739,-0.5));
#4603=CARTESIAN_POINT('Ctrl Pts',(0.288675134594813,0.340908044531739,-0.5));
#4604=CARTESIAN_POINT('Ctrl Pts',(0.433012701893303,0.424241377863696,-0.249999999998124));
#4605=CARTESIAN_POINT('Ctrl Pts',(0.577350269189626,0.340908044531739,0.));
#4606=CARTESIAN_POINT('',(-0.288675134594813,0.340908044531739,-0.5));
#4607=CARTESIAN_POINT('Ctrl Pts',(-0.288675134594813,0.340908044531739,
-0.5));
#4608=CARTESIAN_POINT('Ctrl Pts',(2.16660023255599E-12,0.424241377863696,
-0.5));
#4609=CARTESIAN_POINT('Ctrl Pts',(0.288675134594813,0.340908044531739,-0.5));
#4610=CARTESIAN_POINT('Ctrl Pts',(-0.577350269189626,0.340908044531739,
-7.07050159149938E-17));
#4611=CARTESIAN_POINT('Ctrl Pts',(-0.433012701891136,0.424241377863697,
-0.250000000001876));
#4612=CARTESIAN_POINT('Ctrl Pts',(-0.288675134594813,0.340908044531739,
-0.5));
#4613=CARTESIAN_POINT('Origin',(0.288675134594813,0.,-0.5));
#4614=CARTESIAN_POINT('',(0.288675134594813,0.,-0.5));
#4615=CARTESIAN_POINT('',(0.288675134594813,0.,-0.5));
#4616=CARTESIAN_POINT('',(-0.288675134594813,0.,-0.5));
#4617=CARTESIAN_POINT('',(0.288675134594813,0.,-0.5));
#4618=CARTESIAN_POINT('',(-0.288675134594813,0.,-0.5));
#4619=CARTESIAN_POINT('Origin',(0.577350269189626,0.,0.));
#4620=CARTESIAN_POINT('',(0.577350269189626,0.,0.));
#4621=CARTESIAN_POINT('',(0.577350269189626,0.,0.));
#4622=CARTESIAN_POINT('',(0.577350269189626,0.,0.));
#4623=CARTESIAN_POINT('Origin',(0.288675134594813,0.,0.5));
#4624=CARTESIAN_POINT('',(0.288675134594813,0.,0.5));
#4625=CARTESIAN_POINT('',(0.288675134594813,0.,0.5));
#4626=CARTESIAN_POINT('',(0.288675134594813,0.,0.5));
#4627=CARTESIAN_POINT('Origin',(-0.288675134594813,0.,0.5));
#4628=CARTESIAN_POINT('',(-0.288675134594813,0.,0.5));
#4629=CARTESIAN_POINT('',(-0.288675134594813,0.,0.5));
#4630=CARTESIAN_POINT('',(-0.288675134594813,0.,0.5));
#4631=CARTESIAN_POINT('Origin',(-0.577350269189626,0.,-7.07050159149938E-17));
#4632=CARTESIAN_POINT('',(-0.577350269189626,0.,-7.07050159149938E-17));
#4633=CARTESIAN_POINT('',(-0.577350269189626,0.,-7.07050159149938E-17));
#4634=CARTESIAN_POINT('',(-0.577350269189626,0.,-7.07050159149938E-17));
#4635=CARTESIAN_POINT('Origin',(-0.288675134594813,0.,-0.5));
#4636=CARTESIAN_POINT('',(-0.288675134594813,0.,-0.5));
#4637=CARTESIAN_POINT('Origin',(0.,0.4,0.));
#4638=CARTESIAN_POINT('Origin',(0.,0.,0.));
#4639=CARTESIAN_POINT('',(0.,0.,0.));
#4640=CARTESIAN_POINT('Origin',(14.4,0.,-0.1));
#4641=CARTESIAN_POINT('',(14.125,-3.36777869765523E-17,0.));
#4642=CARTESIAN_POINT('Origin',(14.4,0.,0.));
#4643=CARTESIAN_POINT('',(14.125,3.36777869765523E-17,0.6));
#4644=CARTESIAN_POINT('',(14.125,-3.36777869765523E-17,-0.1));
#4645=CARTESIAN_POINT('Origin',(14.4,0.,0.6));
#4646=CARTESIAN_POINT('Origin',(17.,0.,-0.1));
#4647=CARTESIAN_POINT('',(16.725,-3.3677786976552E-17,0.));
#4648=CARTESIAN_POINT('Origin',(17.,0.,0.));
#4649=CARTESIAN_POINT('',(16.725,3.3677786976552E-17,0.6));
#4650=CARTESIAN_POINT('',(16.725,-3.3677786976552E-17,-0.1));
#4651=CARTESIAN_POINT('Origin',(17.,0.,0.6));
#4652=CARTESIAN_POINT('Origin',(15.3,0.9,2.));
#4653=CARTESIAN_POINT('',(15.59,0.9,3.5));
#4654=CARTESIAN_POINT('',(15.,0.9,3.42318854252131));
#4655=CARTESIAN_POINT('Origin',(15.29,0.9,3.5));
#4656=CARTESIAN_POINT('',(15.,0.9,0.6));
#4657=CARTESIAN_POINT('',(15.,0.9,3.5));
#4658=CARTESIAN_POINT('',(15.6,0.9,0.6));
#4659=CARTESIAN_POINT('',(15.525,0.9,0.6));
#4660=CARTESIAN_POINT('',(15.6,0.9,3.5));
#4661=CARTESIAN_POINT('',(15.6,0.9,0.5));
#4662=CARTESIAN_POINT('',(15.6,0.9,3.5));
#4663=CARTESIAN_POINT('Origin',(15.29,0.9,3.5));
#4664=CARTESIAN_POINT('',(15.,1.3,3.42318854252131));
#4665=CARTESIAN_POINT('',(15.,0.9,3.42318854252131));
#4666=CARTESIAN_POINT('',(15.59,1.3,3.5));
#4667=CARTESIAN_POINT('',(15.59,0.9,3.5));
#4668=CARTESIAN_POINT('',(14.99,1.3,3.5));
#4669=CARTESIAN_POINT('Origin',(15.29,1.3,3.5));
#4670=CARTESIAN_POINT('',(14.99,-1.3,3.5));
#4671=CARTESIAN_POINT('',(14.99,0.9,3.5));
#4672=CARTESIAN_POINT('',(15.59,-1.3,3.5));
#4673=CARTESIAN_POINT('Origin',(15.29,-1.3,3.5));
#4674=CARTESIAN_POINT('',(15.59,-0.9,3.5));
#4675=CARTESIAN_POINT('',(15.59,-1.3,3.5));
#4676=CARTESIAN_POINT('',(15.,-0.9,3.42318854252131));
#4677=CARTESIAN_POINT('Origin',(15.29,-0.9,3.5));
#4678=CARTESIAN_POINT('',(15.,-1.3,3.42318854252131));
#4679=CARTESIAN_POINT('',(15.,-1.3,3.42318854252131));
#4680=CARTESIAN_POINT('Origin',(15.29,-1.3,3.5));
#4681=CARTESIAN_POINT('Origin',(15.29,1.3,3.5));
#4682=CARTESIAN_POINT('Origin',(15.3,1.3,2.));
#4683=CARTESIAN_POINT('',(15.6,1.3,3.5));
#4684=CARTESIAN_POINT('',(15.6,1.3,3.5));
#4685=CARTESIAN_POINT('',(15.6,1.3,0.6));
#4686=CARTESIAN_POINT('',(15.6,1.3,0.5));
#4687=CARTESIAN_POINT('',(15.,1.3,0.6));
#4688=CARTESIAN_POINT('',(15.525,1.3,0.6));
#4689=CARTESIAN_POINT('',(15.,1.3,3.5));
#4690=CARTESIAN_POINT('Origin',(15.,0.9,3.5));
#4691=CARTESIAN_POINT('',(15.6,0.9,3.5));
#4692=CARTESIAN_POINT('Origin',(15.6,0.9,3.5));
#4693=CARTESIAN_POINT('',(15.6,0.45,0.6));
#4694=CARTESIAN_POINT('Origin',(15.,0.9,0.5));
#4695=CARTESIAN_POINT('',(15.,0.45,0.6));
#4696=CARTESIAN_POINT('Origin',(15.3,-0.9,2.));
#4697=CARTESIAN_POINT('',(15.6,-0.9,3.5));
#4698=CARTESIAN_POINT('',(15.6,-0.9,3.5));
#4699=CARTESIAN_POINT('',(15.6,-0.9,0.6));
#4700=CARTESIAN_POINT('',(15.6,-0.9,0.5));
#4701=CARTESIAN_POINT('',(15.,-0.9,0.6));
#4702=CARTESIAN_POINT('',(15.525,-0.9,0.6));
#4703=CARTESIAN_POINT('',(15.,-0.9,3.5));
#4704=CARTESIAN_POINT('Origin',(15.,-1.3,3.5));
#4705=CARTESIAN_POINT('',(15.6,-1.3,3.5));
#4706=CARTESIAN_POINT('',(15.6,-1.3,3.5));
#4707=CARTESIAN_POINT('',(15.6,-1.3,3.5));
#4708=CARTESIAN_POINT('Origin',(15.3,-1.3,2.));
#4709=CARTESIAN_POINT('',(15.,-1.3,0.6));
#4710=CARTESIAN_POINT('',(15.,-1.3,3.5));
#4711=CARTESIAN_POINT('',(15.6,-1.3,0.6));
#4712=CARTESIAN_POINT('',(15.525,-1.3,0.6));
#4713=CARTESIAN_POINT('',(15.6,-1.3,0.5));
#4714=CARTESIAN_POINT('Origin',(15.6,-1.3,3.5));
#4715=CARTESIAN_POINT('',(15.6,-0.65,0.6));
#4716=CARTESIAN_POINT('Origin',(15.,-1.3,0.5));
#4717=CARTESIAN_POINT('',(15.,-0.65,0.6));
#4718=CARTESIAN_POINT('Origin',(17.5,1.8,0.));
#4719=CARTESIAN_POINT('',(17.5,1.8,0.));
#4720=CARTESIAN_POINT('',(14.,1.8,0.));
#4721=CARTESIAN_POINT('',(17.5,1.8,0.));
#4722=CARTESIAN_POINT('',(14.,1.8,0.6));
#4723=CARTESIAN_POINT('',(14.,1.8,0.));
#4724=CARTESIAN_POINT('',(17.5,1.8,0.6));
#4725=CARTESIAN_POINT('',(17.5,1.8,0.6));
#4726=CARTESIAN_POINT('',(17.5,1.8,0.));
#4727=CARTESIAN_POINT('Origin',(17.5,-1.8,0.));
#4728=CARTESIAN_POINT('',(17.5,-1.8,0.));
#4729=CARTESIAN_POINT('',(17.5,-1.8,0.));
#4730=CARTESIAN_POINT('',(17.5,-1.8,0.6));
#4731=CARTESIAN_POINT('',(17.5,-1.8,0.6));
#4732=CARTESIAN_POINT('',(17.5,-1.8,0.));
#4733=CARTESIAN_POINT('Origin',(14.,-1.8,0.));
#4734=CARTESIAN_POINT('',(14.,-1.8,0.));
#4735=CARTESIAN_POINT('',(14.,-1.8,0.));
#4736=CARTESIAN_POINT('',(14.,-1.8,0.6));
#4737=CARTESIAN_POINT('',(14.,-1.8,0.6));
#4738=CARTESIAN_POINT('',(14.,-1.8,0.));
#4739=CARTESIAN_POINT('Origin',(14.,1.8,0.));
#4740=CARTESIAN_POINT('',(14.,1.8,0.));
#4741=CARTESIAN_POINT('',(14.,1.8,0.6));
#4742=CARTESIAN_POINT('Origin',(15.75,0.,0.6));
#4743=CARTESIAN_POINT('Origin',(15.75,0.,0.));
#4744=CARTESIAN_POINT('',(0.,0.,0.));
#4745=CARTESIAN_POINT('',(0.,0.,0.));
#4746=CARTESIAN_POINT('Origin',(-5.97716818855047,-0.5,1.97706554351405));
#4747=CARTESIAN_POINT('',(-6.25216818855047,-0.4,1.97706554351405));
#4748=CARTESIAN_POINT('Origin',(-5.97716818855047,-0.4,1.97706554351405));
#4749=CARTESIAN_POINT('',(-6.25216818855047,0.4,1.97706554351405));
#4750=CARTESIAN_POINT('',(-6.25216818855047,-0.5,1.97706554351405));
#4751=CARTESIAN_POINT('Origin',(-5.97716818855047,0.4,1.97706554351405));
#4752=CARTESIAN_POINT('Origin',(0.,-0.5,2.5));
#4753=CARTESIAN_POINT('',(-0.31,-0.4,2.5));
#4754=CARTESIAN_POINT('Origin',(0.,-0.4,2.5));
#4755=CARTESIAN_POINT('',(-0.31,0.4,2.5));
#4756=CARTESIAN_POINT('',(-0.31,-0.5,2.5));
#4757=CARTESIAN_POINT('Origin',(0.,0.4,2.5));
#4758=CARTESIAN_POINT('Origin',(-2.49048674522936,-0.5,2.28211064313086));
#4759=CARTESIAN_POINT('',(-2.80048674522936,-0.4,2.28211064313086));
#4760=CARTESIAN_POINT('Origin',(-2.49048674522936,-0.4,2.28211064313086));
#4761=CARTESIAN_POINT('',(-2.80048674522936,0.4,2.28211064313086));
#4762=CARTESIAN_POINT('',(-2.80048674522936,-0.5,2.28211064313086));
#4763=CARTESIAN_POINT('Origin',(-2.49048674522936,0.4,2.28211064313086));
#4764=CARTESIAN_POINT('Origin',(-5.97716818855047,-0.4,1.97706554351405));
#4765=CARTESIAN_POINT('',(-5.56651867289793,0.4,2.4145206558334));
#4766=CARTESIAN_POINT('',(-5.56651867289793,-0.4,2.4145206558334));
#4767=CARTESIAN_POINT('',(-5.56651867289793,-0.4,2.4145206558334));
#4768=CARTESIAN_POINT('',(-5.49679407869981,0.4,1.61756489736));
#4769=CARTESIAN_POINT('Origin',(-5.97716818855047,0.4,1.97706554351405));
#4770=CARTESIAN_POINT('',(-5.49679407869981,-0.4,1.61756489736));
#4771=CARTESIAN_POINT('',(-5.49679407869981,-0.4,1.61756489736));
#4772=CARTESIAN_POINT('Origin',(-5.97716818855047,-0.4,1.97706554351405));
#4773=CARTESIAN_POINT('Origin',(0.,-0.4,2.5));
#4774=CARTESIAN_POINT('',(-2.90113626088191,-0.4,1.84465553081151));
#4775=CARTESIAN_POINT('',(0.0348622970990632,-0.4,2.1015221207633));
#4776=CARTESIAN_POINT('',(-2.0101126353787,-0.4,1.92260999697681));
#4777=CARTESIAN_POINT('Origin',(-2.49048674522936,-0.4,2.28211064313086));
#4778=CARTESIAN_POINT('',(-0.410649515652541,-0.4,2.06254488768065));
#4779=CARTESIAN_POINT('',(0.0348622970990632,-0.4,2.1015221207633));
#4780=CARTESIAN_POINT('',(-0.480374109850668,-0.4,2.85950064615405));
#4781=CARTESIAN_POINT('Origin',(0.,-0.4,2.5));
#4782=CARTESIAN_POINT('',(-2.07983722957682,-0.4,2.7195657554502));
#4783=CARTESIAN_POINT('',(-6.01203048564954,-0.4,2.37554342275075));
#4784=CARTESIAN_POINT('',(-2.97086085508003,-0.4,2.6416112892849));
#4785=CARTESIAN_POINT('Origin',(-2.49048674522936,-0.4,2.28211064313086));
#4786=CARTESIAN_POINT('',(-6.01203048564954,-0.4,2.37554342275075));
#4787=CARTESIAN_POINT('Origin',(0.0348622970990632,-0.4,2.1015221207633));
#4788=CARTESIAN_POINT('',(-2.90113626088191,0.4,1.84465553081151));
#4789=CARTESIAN_POINT('',(0.0348622970990632,0.4,2.1015221207633));
#4790=CARTESIAN_POINT('',(-2.90113626088191,-0.4,1.84465553081151));
#4791=CARTESIAN_POINT('Origin',(-2.49048674522936,-0.4,2.28211064313086));
#4792=CARTESIAN_POINT('',(-2.0101126353787,0.4,1.92260999697681));
#4793=CARTESIAN_POINT('Origin',(-2.49048674522936,0.4,2.28211064313086));
#4794=CARTESIAN_POINT('',(-2.0101126353787,-0.4,1.92260999697681));
#4795=CARTESIAN_POINT('Origin',(-2.49048674522936,-0.4,2.28211064313086));
#4796=CARTESIAN_POINT('',(-2.97086085508003,0.4,2.6416112892849));
#4797=CARTESIAN_POINT('',(-2.97086085508003,-0.4,2.6416112892849));
#4798=CARTESIAN_POINT('',(-2.07983722957682,0.4,2.7195657554502));
#4799=CARTESIAN_POINT('',(-2.07983722957682,-0.4,2.7195657554502));
#4800=CARTESIAN_POINT('Origin',(-2.49048674522936,0.4,2.28211064313086));
#4801=CARTESIAN_POINT('Origin',(0.,0.4,2.5));
#4802=CARTESIAN_POINT('',(-6.01203048564954,0.4,2.37554342275075));
#4803=CARTESIAN_POINT('',(-0.480374109850668,0.4,2.85950064615405));
#4804=CARTESIAN_POINT('',(-6.01203048564954,0.4,2.37554342275075));
#4805=CARTESIAN_POINT('',(-0.410649515652541,0.4,2.06254488768065));
#4806=CARTESIAN_POINT('Origin',(0.,0.4,2.5));
#4807=CARTESIAN_POINT('',(0.0348622970990632,0.4,2.1015221207633));
#4808=CARTESIAN_POINT('Origin',(-6.01203048564954,-0.4,2.37554342275075));
#4809=CARTESIAN_POINT('',(-0.480374109850667,-0.4,2.85950064615405));
#4810=CARTESIAN_POINT('Origin',(0.0348622970990632,-0.4,2.1015221207633));
#4811=CARTESIAN_POINT('',(-0.410649515652541,-0.4,2.06254488768065));
#4812=CARTESIAN_POINT('Origin',(-6.01203048564954,-0.4,2.37554342275075));
#4813=CARTESIAN_POINT('Origin',(0.,-0.4,2.5));
#4814=CARTESIAN_POINT('',(0.,0.,0.));
#4815=CARTESIAN_POINT('Origin',(-2.49048674522936,-0.74,2.28211064313086));
#4816=CARTESIAN_POINT('',(-2.80048674522936,-0.56,2.28211064313086));
#4817=CARTESIAN_POINT('Origin',(-2.49048674522936,-0.56,2.28211064313086));
#4818=CARTESIAN_POINT('',(-2.80048674522936,-0.74,2.28211064313086));
#4819=CARTESIAN_POINT('',(-2.80048674522936,-0.74,2.28211064313086));
#4820=CARTESIAN_POINT('Origin',(-2.49048674522936,-0.74,2.28211064313086));
#4821=CARTESIAN_POINT('Origin',(-2.49048674522936,-0.74,2.28211064313086));
#4822=CARTESIAN_POINT('',(-2.89048674522936,-0.56,2.28211064313086));
#4823=CARTESIAN_POINT('Origin',(-2.49048674522936,-0.56,2.28211064313086));
#4824=CARTESIAN_POINT('',(-2.89048674522936,-0.74,2.28211064313086));
#4825=CARTESIAN_POINT('',(-2.89048674522936,-0.74,2.28211064313086));
#4826=CARTESIAN_POINT('Origin',(-2.49048674522936,-0.74,2.28211064313086));
#4827=CARTESIAN_POINT('Origin',(-2.49048674522936,-0.56,2.28211064313086));
#4828=CARTESIAN_POINT('Origin',(-2.49048674522936,-0.74,2.28211064313086));
#4829=CARTESIAN_POINT('',(0.,0.,0.));
#4830=CARTESIAN_POINT('Origin',(-2.49048674522936,0.4,2.28211064313086));
#4831=CARTESIAN_POINT('',(-2.80048674522936,1.1,2.28211064313086));
#4832=CARTESIAN_POINT('Origin',(-2.49048674522936,1.1,2.28211064313086));
#4833=CARTESIAN_POINT('',(-2.80048674522936,0.4,2.28211064313086));
#4834=CARTESIAN_POINT('',(-2.80048674522936,0.4,2.28211064313086));
#4835=CARTESIAN_POINT('Origin',(-2.49048674522936,0.4,2.28211064313086));
#4836=CARTESIAN_POINT('Origin',(-2.49048674522936,0.4,2.28211064313086));
#4837=CARTESIAN_POINT('',(-2.89048674522936,1.1,2.28211064313086));
#4838=CARTESIAN_POINT('Origin',(-2.49048674522936,1.1,2.28211064313086));
#4839=CARTESIAN_POINT('',(-2.89048674522936,0.4,2.28211064313086));
#4840=CARTESIAN_POINT('',(-2.89048674522936,0.4,2.28211064313086));
#4841=CARTESIAN_POINT('Origin',(-2.49048674522936,0.4,2.28211064313086));
#4842=CARTESIAN_POINT('Origin',(-2.49048674522936,1.1,2.28211064313086));
#4843=CARTESIAN_POINT('Origin',(-2.49048674522936,0.4,2.28211064313086));
#4844=CARTESIAN_POINT('',(0.,0.,0.));
#4845=CARTESIAN_POINT('Origin',(0.,-7.7,10.03));
#4846=CARTESIAN_POINT('',(-0.21,-7.7,10.03));
#4847=CARTESIAN_POINT('Origin',(0.,-7.7,10.03));
#4848=CARTESIAN_POINT('',(-0.21,-6.5,10.03));
#4849=CARTESIAN_POINT('',(-0.21,-7.7,10.03));
#4850=CARTESIAN_POINT('Origin',(0.,-6.5,10.03));
#4851=CARTESIAN_POINT('Origin',(0.,-7.7,10.03));
#4852=CARTESIAN_POINT('Origin',(0.,-9.5,10.03));
#4853=CARTESIAN_POINT('',(-0.7,-6.5,10.03));
#4854=CARTESIAN_POINT('Origin',(0.,-6.5,10.03));
#4855=CARTESIAN_POINT('',(-0.7,-9.5,10.03));
#4856=CARTESIAN_POINT('',(-0.7,-9.5,10.03));
#4857=CARTESIAN_POINT('Origin',(0.,-9.5,10.03));
#4858=CARTESIAN_POINT('Origin',(0.,-6.5,10.03));
#4859=CARTESIAN_POINT('Origin',(0.,-9.5,10.03));
#4860=CARTESIAN_POINT('',(0.,0.,0.));
#4861=CARTESIAN_POINT('Origin',(0.115470053837925,-0.5,-0.2));
#4862=CARTESIAN_POINT('',(0.23094010767585,-0.5,0.));
#4863=CARTESIAN_POINT('',(0.115470053837925,-0.5,-0.2));
#4864=CARTESIAN_POINT('',(0.23094010767585,-0.5,0.));
#4865=CARTESIAN_POINT('',(0.115470053837925,-0.8,-0.2));
#4866=CARTESIAN_POINT('',(0.115470053837925,-0.5,-0.2));
#4867=CARTESIAN_POINT('',(0.23094010767585,-0.8,0.));
#4868=CARTESIAN_POINT('',(0.23094010767585,-0.8,0.));
#4869=CARTESIAN_POINT('',(0.23094010767585,-0.5,0.));
#4870=CARTESIAN_POINT('Origin',(-0.115470053837925,-0.5,-0.2));
#4871=CARTESIAN_POINT('',(-0.115470053837925,-0.5,-0.2));
#4872=CARTESIAN_POINT('',(0.115470053837925,-0.5,-0.2));
#4873=CARTESIAN_POINT('',(-0.115470053837925,-0.8,-0.2));
#4874=CARTESIAN_POINT('',(-0.115470053837925,-0.5,-0.2));
#4875=CARTESIAN_POINT('',(0.115470053837925,-0.8,-0.2));
#4876=CARTESIAN_POINT('Origin',(-0.23094010767585,-0.5,-2.77555756156289E-17));
#4877=CARTESIAN_POINT('',(-0.23094010767585,-0.5,-2.82820063659975E-17));
#4878=CARTESIAN_POINT('',(-0.115470053837925,-0.5,-0.2));
#4879=CARTESIAN_POINT('',(-0.23094010767585,-0.8,-2.77555756156289E-17));
#4880=CARTESIAN_POINT('',(-0.23094010767585,-0.5,-2.82820063659975E-17));
#4881=CARTESIAN_POINT('',(-0.115470053837925,-0.8,-0.2));
#4882=CARTESIAN_POINT('Origin',(-0.115470053837925,-0.5,0.2));
#4883=CARTESIAN_POINT('',(-0.115470053837925,-0.5,0.2));
#4884=CARTESIAN_POINT('',(-0.23094010767585,-0.5,-2.82820063659975E-17));
#4885=CARTESIAN_POINT('',(-0.115470053837925,-0.8,0.2));
#4886=CARTESIAN_POINT('',(-0.115470053837925,-0.5,0.2));
#4887=CARTESIAN_POINT('',(-0.23094010767585,-0.8,-2.82820063659975E-17));
#4888=CARTESIAN_POINT('Origin',(0.115470053837925,-0.5,0.2));
#4889=CARTESIAN_POINT('',(0.115470053837925,-0.5,0.2));
#4890=CARTESIAN_POINT('',(-0.115470053837925,-0.5,0.2));
#4891=CARTESIAN_POINT('',(0.115470053837925,-0.8,0.2));
#4892=CARTESIAN_POINT('',(0.115470053837925,-0.5,0.2));
#4893=CARTESIAN_POINT('',(-0.115470053837925,-0.8,0.2));
#4894=CARTESIAN_POINT('Origin',(0.23094010767585,-0.5,0.));
#4895=CARTESIAN_POINT('',(0.115470053837925,-0.5,0.2));
#4896=CARTESIAN_POINT('',(0.115470053837925,-0.8,0.2));
#4897=CARTESIAN_POINT('Origin',(0.,-0.5,0.));
#4898=CARTESIAN_POINT('Origin',(0.,-0.8,0.));
#4899=CARTESIAN_POINT('Origin',(0.,-1.4,0.));
#4900=CARTESIAN_POINT('',(-0.24505,-1.4,3.00099698131059E-17));
#4901=CARTESIAN_POINT('Origin',(0.,-1.4,0.));
#4902=CARTESIAN_POINT('Origin',(0.375,0.5,0.));
#4903=CARTESIAN_POINT('',(-0.375,0.5,-4.59242549680257E-17));
#4904=CARTESIAN_POINT('Origin',(0.,0.5,0.));
#4905=CARTESIAN_POINT('Origin',(0.,0.475,0.));
#4906=CARTESIAN_POINT('',(-0.425,0.45,-5.20474889637625E-17));
#4907=CARTESIAN_POINT('Origin',(0.,0.45,0.));
#4908=CARTESIAN_POINT('',(-0.4,0.475,-4.89858719658941E-17));
#4909=CARTESIAN_POINT('Origin',(0.,0.24,0.));
#4910=CARTESIAN_POINT('',(-0.425,0.0299999999999998,-5.20474889637625E-17));
#4911=CARTESIAN_POINT('Origin',(0.,0.0299999999999998,0.));
#4912=CARTESIAN_POINT('',(-0.425,0.24,-5.20474889637625E-17));
#4913=CARTESIAN_POINT('Origin',(0.,0.0150000000000001,0.));
#4914=CARTESIAN_POINT('',(-0.395,4.85722573273506E-17,-4.83735485663204E-17));
#4915=CARTESIAN_POINT('Origin',(0.,0.,0.));
#4916=CARTESIAN_POINT('',(-0.41,0.0150000000000001,-5.02105187650415E-17));
#4917=CARTESIAN_POINT('Origin',(0.27,0.,0.));
#4918=CARTESIAN_POINT('',(-0.27,0.,-3.30654635769785E-17));
#4919=CARTESIAN_POINT('Origin',(0.,0.,0.));
#4920=CARTESIAN_POINT('Origin',(0.,-0.02,0.));
#4921=CARTESIAN_POINT('',(-0.24505,-0.0498999999999999,3.00099698131059E-17));
#4922=CARTESIAN_POINT('Origin',(0.,-0.0498999999999999,0.));
#4923=CARTESIAN_POINT('',(-0.26,-0.02,-3.18408167778312E-17));
#4924=CARTESIAN_POINT('Origin',(0.,-0.995,0.));
#4925=CARTESIAN_POINT('',(-0.24505,-0.995,-3.00099698131059E-17));
#4926=CARTESIAN_POINT('',(0.,0.,0.));
#4927=CARTESIAN_POINT('',(0.,0.,0.));
#4928=CARTESIAN_POINT('Origin',(-2.49048674522936,1.,2.28211064313086));
#4929=CARTESIAN_POINT('',(-2.80048674522936,1.1,2.28211064313086));
#4930=CARTESIAN_POINT('Origin',(-2.49048674522936,1.1,2.28211064313086));
#4931=CARTESIAN_POINT('',(-2.80048674522936,1.7,2.28211064313086));
#4932=CARTESIAN_POINT('',(-2.80048674522936,1.,2.28211064313086));
#4933=CARTESIAN_POINT('Origin',(-2.49048674522936,1.7,2.28211064313086));
#4934=CARTESIAN_POINT('Origin',(2.00423507354465,1.,2.5));
#4935=CARTESIAN_POINT('',(1.69423507354465,1.1,2.5));
#4936=CARTESIAN_POINT('Origin',(2.00423507354465,1.1,2.5));
#4937=CARTESIAN_POINT('',(1.69423507354465,1.7,2.5));
#4938=CARTESIAN_POINT('',(1.69423507354465,1.,2.5));
#4939=CARTESIAN_POINT('Origin',(2.00423507354465,1.7,2.5));
#4940=CARTESIAN_POINT('Origin',(2.00423507354465,1.1,2.5));
#4941=CARTESIAN_POINT('',(1.57691397074501,1.7,2.07881515328528));
#4942=CARTESIAN_POINT('',(1.57691397074501,1.1,2.07881515328528));
#4943=CARTESIAN_POINT('',(1.57691397074501,1.1,2.07881515328528));
#4944=CARTESIAN_POINT('',(1.53817808507938,1.7,2.87787680995622));
#4945=CARTESIAN_POINT('Origin',(2.00423507354465,1.7,2.5));
#4946=CARTESIAN_POINT('',(1.53817808507938,1.1,2.87787680995622));
#4947=CARTESIAN_POINT('',(1.53817808507938,1.1,2.87787680995622));
#4948=CARTESIAN_POINT('Origin',(2.00423507354465,1.1,2.5));
#4949=CARTESIAN_POINT('Origin',(2.02360301637746,1.1,2.10046917166453));
#4950=CARTESIAN_POINT('',(-2.0244297567641,1.1,1.90423383317464));
#4951=CARTESIAN_POINT('',(2.02360301637746,1.1,2.10046917166453));
#4952=CARTESIAN_POINT('',(-2.0244297567641,1.7,1.90423383317464));
#4953=CARTESIAN_POINT('',(-2.0244297567641,1.1,1.90423383317464));
#4954=CARTESIAN_POINT('',(2.02360301637746,1.7,2.10046917166453));
#4955=CARTESIAN_POINT('Origin',(-2.49048674522936,1.1,2.28211064313086));
#4956=CARTESIAN_POINT('',(-2.06316564242972,1.1,2.70329548984557));
#4957=CARTESIAN_POINT('',(-2.50985468806218,1.1,2.68164147146632));
#4958=CARTESIAN_POINT('Origin',(-2.49048674522936,1.1,2.28211064313086));
#4959=CARTESIAN_POINT('Origin',(-2.50985468806218,1.1,2.68164147146632));
#4960=CARTESIAN_POINT('',(-2.06316564242972,1.7,2.70329548984557));
#4961=CARTESIAN_POINT('',(-2.50985468806218,1.7,2.68164147146632));
#4962=CARTESIAN_POINT('',(-2.06316564242972,1.1,2.70329548984557));
#4963=CARTESIAN_POINT('Origin',(-2.49048674522936,1.1,2.28211064313086));
#4964=CARTESIAN_POINT('Origin',(-2.49048674522936,1.7,2.28211064313086));
#4965=CARTESIAN_POINT('Origin',(-2.49048674522936,1.7,2.28211064313086));
#4966=CARTESIAN_POINT('',(0.,0.,0.));
#4967=CARTESIAN_POINT('',(0.,0.,0.));
#4968=CARTESIAN_POINT('',(0.,0.,0.));
#4969=CARTESIAN_POINT('Origin',(9.9,0.,2.5));
#4970=CARTESIAN_POINT('',(9.9,-4.163799117101E-17,2.84));
#4971=CARTESIAN_POINT('Origin',(9.9,0.,2.5));
#4972=CARTESIAN_POINT('',(11.,4.163799117101E-17,2.84));
#4973=CARTESIAN_POINT('',(9.9,-4.163799117101E-17,2.84));
#4974=CARTESIAN_POINT('Origin',(11.,0.,2.5));
#4975=CARTESIAN_POINT('Origin',(9.9,0.,2.5));
#4976=CARTESIAN_POINT('Origin',(9.9,-1.5,2.5));
#4977=CARTESIAN_POINT('',(10.,-1.5,2.925));
#4978=CARTESIAN_POINT('Origin',(10.,-1.5,2.5));
#4979=CARTESIAN_POINT('',(11.,-1.5,2.925));
#4980=CARTESIAN_POINT('',(9.9,-1.5,2.925));
#4981=CARTESIAN_POINT('Origin',(11.,-1.5,2.5));
#4982=CARTESIAN_POINT('Origin',(9.9,1.5,2.5));
#4983=CARTESIAN_POINT('',(10.,1.5,2.925));
#4984=CARTESIAN_POINT('Origin',(10.,1.5,2.5));
#4985=CARTESIAN_POINT('',(11.,1.5,2.925));
#4986=CARTESIAN_POINT('',(9.9,1.5,2.925));
#4987=CARTESIAN_POINT('Origin',(11.,1.5,2.5));
#4988=CARTESIAN_POINT('Origin',(10.,0.,2.5));
#4989=CARTESIAN_POINT('',(10.,-2.4,3.3));
#4990=CARTESIAN_POINT('',(10.,-2.4,1.7));
#4991=CARTESIAN_POINT('',(10.,-2.4,3.3));
#4992=CARTESIAN_POINT('',(10.,2.4,3.3));
#4993=CARTESIAN_POINT('',(10.,2.4,3.3));
#4994=CARTESIAN_POINT('',(10.,2.4,1.7));
#4995=CARTESIAN_POINT('',(10.,2.4,1.7));
#4996=CARTESIAN_POINT('',(10.,-2.4,1.7));
#4997=CARTESIAN_POINT('',(10.,-7.34788079488412E-17,3.1));
#4998=CARTESIAN_POINT('Origin',(10.,0.,2.5));
#4999=CARTESIAN_POINT('Origin',(10.,2.4,3.3));
#5000=CARTESIAN_POINT('',(11.,-2.4,3.3));
#5001=CARTESIAN_POINT('',(10.,-2.4,3.3));
#5002=CARTESIAN_POINT('',(11.,2.4,3.3));
#5003=CARTESIAN_POINT('',(11.,2.4,3.3));
#5004=CARTESIAN_POINT('',(10.,2.4,3.3));
#5005=CARTESIAN_POINT('Origin',(10.,2.4,1.7));
#5006=CARTESIAN_POINT('',(11.,2.4,1.7));
#5007=CARTESIAN_POINT('',(11.,2.4,1.7));
#5008=CARTESIAN_POINT('',(10.,2.4,1.7));
#5009=CARTESIAN_POINT('Origin',(10.,-2.4,1.7));
#5010=CARTESIAN_POINT('',(11.,-2.4,1.7));
#5011=CARTESIAN_POINT('',(11.,-2.4,1.7));
#5012=CARTESIAN_POINT('',(10.,-2.4,1.7));
#5013=CARTESIAN_POINT('Origin',(10.,-2.4,3.3));
#5014=CARTESIAN_POINT('',(11.,-2.4,3.3));
#5015=CARTESIAN_POINT('Origin',(11.,0.,2.5));
#5016=CARTESIAN_POINT('Origin',(2.00423507354465,1.6,2.5));
#5017=CARTESIAN_POINT('',(1.69423507354465,1.72,2.5));
#5018=CARTESIAN_POINT('Origin',(2.00423507354465,1.72,2.5));
#5019=CARTESIAN_POINT('',(1.69423507354465,2.12,2.5));
#5020=CARTESIAN_POINT('',(1.69423507354465,1.6,2.5));
#5021=CARTESIAN_POINT('Origin',(2.00423507354465,2.12,2.5));
#5022=CARTESIAN_POINT('Origin',(2.00423507354465,1.72,2.5));
#5023=CARTESIAN_POINT('',(2.00423507354465,1.72,3.1));
#5024=CARTESIAN_POINT('',(2.00423507354465,2.12,3.1));
#5025=CARTESIAN_POINT('',(2.00423507354465,1.72,3.1));
#5026=CARTESIAN_POINT('',(2.00423507354465,2.12,1.9));
#5027=CARTESIAN_POINT('Origin',(2.00423507354465,2.12,2.5));
#5028=CARTESIAN_POINT('',(2.00423507354465,1.72,1.9));
#5029=CARTESIAN_POINT('',(2.00423507354465,1.72,1.9));
#5030=CARTESIAN_POINT('Origin',(2.00423507354465,1.72,2.5));
#5031=CARTESIAN_POINT('Origin',(3.00211753677232,1.72,2.5));
#5032=CARTESIAN_POINT('',(3.,1.72,1.9));
#5033=CARTESIAN_POINT('',(2.00423507354465,1.72,1.9));
#5034=CARTESIAN_POINT('',(3.,1.72,3.1));
#5035=CARTESIAN_POINT('',(3.,1.72,2.2));
#5036=CARTESIAN_POINT('',(4.,1.72,3.1));
#5037=CARTESIAN_POINT('Origin',(3.,0.,1.9));
#5038=CARTESIAN_POINT('',(3.,0.,1.9));
#5039=CARTESIAN_POINT('',(3.,0.,1.9));
#5040=CARTESIAN_POINT('',(3.,0.,3.1));
#5041=CARTESIAN_POINT('',(3.,0.,3.1));
#5042=CARTESIAN_POINT('',(3.,0.,3.1));
#5043=CARTESIAN_POINT('Origin',(3.5,0.,2.5));
#5044=CARTESIAN_POINT('',(4.,-7.34788079488412E-17,3.1));
#5045=CARTESIAN_POINT('',(4.,0.,3.1));
#5046=CARTESIAN_POINT('',(4.,0.,1.9));
#5047=CARTESIAN_POINT('',(3.,0.,1.9));
#5048=CARTESIAN_POINT('',(4.,0.,2.5));
#5049=CARTESIAN_POINT('Origin',(4.,1.72,1.9));
#5050=CARTESIAN_POINT('',(4.,2.12,1.9));
#5051=CARTESIAN_POINT('',(2.00423507354465,2.12,1.9));
#5052=CARTESIAN_POINT('',(4.,1.72,1.9));
#5053=CARTESIAN_POINT('Origin',(2.00423507354465,1.72,3.1));
#5054=CARTESIAN_POINT('',(4.,2.12,3.1));
#5055=CARTESIAN_POINT('',(4.,2.12,3.1));
#5056=CARTESIAN_POINT('',(4.,1.72,3.1));
#5057=CARTESIAN_POINT('Origin',(4.,1.72,3.1));
#5058=CARTESIAN_POINT('',(4.,2.12,1.9));
#5059=CARTESIAN_POINT('Origin',(4.,0.,2.5));
#5060=CARTESIAN_POINT('Origin',(3.00211753677232,2.12,2.5));
#5061=CARTESIAN_POINT('Origin',(4.,0.,2.5));
#5062=CARTESIAN_POINT('Origin',(4.,0.,2.5));
#5063=CARTESIAN_POINT('Origin',(4.,0.,2.5));
#5064=CARTESIAN_POINT('',(4.,-7.34788079488412E-17,3.1));
#5065=CARTESIAN_POINT('',(0.,0.,0.));
#5066=CARTESIAN_POINT('Origin',(2.00423507354465,-0.32,2.5));
#5067=CARTESIAN_POINT('',(1.69423507354465,0.94,2.5));
#5068=CARTESIAN_POINT('Origin',(2.00423507354465,0.94,2.5));
#5069=CARTESIAN_POINT('',(1.69423507354465,-0.32,2.5));
#5070=CARTESIAN_POINT('',(1.69423507354465,-0.32,2.5));
#5071=CARTESIAN_POINT('Origin',(2.00423507354465,-0.32,2.5));
#5072=CARTESIAN_POINT('Origin',(2.00423507354465,-0.32,2.5));
#5073=CARTESIAN_POINT('',(1.60423507354465,0.94,2.5));
#5074=CARTESIAN_POINT('Origin',(2.00423507354465,0.94,2.5));
#5075=CARTESIAN_POINT('',(1.60423507354465,-0.32,2.5));
#5076=CARTESIAN_POINT('',(1.60423507354465,-0.32,2.5));
#5077=CARTESIAN_POINT('Origin',(2.00423507354465,-0.32,2.5));
#5078=CARTESIAN_POINT('Origin',(2.00423507354465,0.94,2.5));
#5079=CARTESIAN_POINT('Origin',(2.00423507354465,-0.32,2.5));
#5080=CARTESIAN_POINT('',(0.,0.,0.));
#5081=CARTESIAN_POINT('Origin',(0.,-2.7,0.));
#5082=CARTESIAN_POINT('',(-0.289136645896019,-2.7,0.08));
#5083=CARTESIAN_POINT('',(-0.3,-2.78,-2.27065106771523E-17));
#5084=CARTESIAN_POINT('Ctrl Pts',(-0.289136645896019,-2.7,0.08));
#5085=CARTESIAN_POINT('Ctrl Pts',(-0.289136645896019,-2.71009877520201,
0.08));
#5086=CARTESIAN_POINT('Ctrl Pts',(-0.289720927595908,-2.72083518625944,
0.0779717130936404));
#5087=CARTESIAN_POINT('Ctrl Pts',(-0.291799203044223,-2.74052980652726,
0.0697927537456149));
#5088=CARTESIAN_POINT('Ctrl Pts',(-0.293259762986909,-2.74949254880105,
0.0636445361887959));
#5089=CARTESIAN_POINT('Ctrl Pts',(-0.295976783522942,-2.76364324458222,
0.0494938404076284));
#5090=CARTESIAN_POINT('Ctrl Pts',(-0.297414335384467,-2.76979246713824,
0.0405305642602551));
#5091=CARTESIAN_POINT('Ctrl Pts',(-0.299439403644655,-2.77797216257078,
0.0208340363410407));
#5092=CARTESIAN_POINT('Ctrl Pts',(-0.3,-2.78,0.0100969318362556));
#5093=CARTESIAN_POINT('Ctrl Pts',(-0.3,-2.78,5.20417042793042E-18));
#5094=CARTESIAN_POINT('',(0.289136645896019,-2.7,0.08));
#5095=CARTESIAN_POINT('',(0.,-2.7,0.08));
#5096=CARTESIAN_POINT('Ctrl Pts',(0.289136645896019,-2.7,0.08));
#5097=CARTESIAN_POINT('Ctrl Pts',(0.289136645896019,-2.68990122479799,0.08));
#5098=CARTESIAN_POINT('Ctrl Pts',(0.289720927595908,-2.67916481374056,0.0779717130936404));
#5099=CARTESIAN_POINT('Ctrl Pts',(0.291799203044223,-2.65947019347274,0.0697927537456147));
#5100=CARTESIAN_POINT('Ctrl Pts',(0.293259762986909,-2.65050745119895,0.0636445361887959));
#5101=CARTESIAN_POINT('Ctrl Pts',(0.295976783522942,-2.63635675541778,0.0494938404076283));
#5102=CARTESIAN_POINT('Ctrl Pts',(0.297414335384467,-2.63020753286176,0.0405305642602551));
#5103=CARTESIAN_POINT('Ctrl Pts',(0.299439403644655,-2.62202783742922,0.0208340363410406));
#5104=CARTESIAN_POINT('Ctrl Pts',(0.3,-2.62,0.0100969318362555));
#5105=CARTESIAN_POINT('Ctrl Pts',(0.3,-2.62,-0.0100969318362556));
#5106=CARTESIAN_POINT('Ctrl Pts',(0.299439403644655,-2.62202783742922,-0.0208340363410406));
#5107=CARTESIAN_POINT('Ctrl Pts',(0.297414335384467,-2.63020753286176,-0.0405305642602551));
#5108=CARTESIAN_POINT('Ctrl Pts',(0.295976783522942,-2.63635675541778,-0.0494938404076283));
#5109=CARTESIAN_POINT('Ctrl Pts',(0.293259762986909,-2.65050745119895,-0.0636445361887959));
#5110=CARTESIAN_POINT('Ctrl Pts',(0.291799203044223,-2.65947019347274,-0.0697927537456147));
#5111=CARTESIAN_POINT('Ctrl Pts',(0.289720927595908,-2.67916481374056,-0.0779717130936403));
#5112=CARTESIAN_POINT('Ctrl Pts',(0.289136645896019,-2.68990122479799,-0.08));
#5113=CARTESIAN_POINT('Ctrl Pts',(0.289136645896019,-2.71009877520201,-0.08));
#5114=CARTESIAN_POINT('Ctrl Pts',(0.289720927595908,-2.72083518625944,-0.0779717130936404));
#5115=CARTESIAN_POINT('Ctrl Pts',(0.291799203044223,-2.74052980652726,-0.0697927537456147));
#5116=CARTESIAN_POINT('Ctrl Pts',(0.293259762986909,-2.74949254880105,-0.0636445361887959));
#5117=CARTESIAN_POINT('Ctrl Pts',(0.295976783522942,-2.76364324458222,-0.0494938404076283));
#5118=CARTESIAN_POINT('Ctrl Pts',(0.297414335384467,-2.76979246713824,-0.0405305642602551));
#5119=CARTESIAN_POINT('Ctrl Pts',(0.299439403644655,-2.77797216257078,-0.0208340363410406));
#5120=CARTESIAN_POINT('Ctrl Pts',(0.3,-2.78,-0.0100969318362555));
#5121=CARTESIAN_POINT('Ctrl Pts',(0.3,-2.78,0.0100969318362556));
#5122=CARTESIAN_POINT('Ctrl Pts',(0.299439403644655,-2.77797216257078,0.0208340363410407));
#5123=CARTESIAN_POINT('Ctrl Pts',(0.297414335384467,-2.76979246713824,0.0405305642602551));
#5124=CARTESIAN_POINT('Ctrl Pts',(0.295976783522942,-2.76364324458222,0.0494938404076284));
#5125=CARTESIAN_POINT('Ctrl Pts',(0.293259762986909,-2.74949254880105,0.0636445361887959));
#5126=CARTESIAN_POINT('Ctrl Pts',(0.291799203044223,-2.74052980652726,0.0697927537456149));
#5127=CARTESIAN_POINT('Ctrl Pts',(0.289720927595908,-2.72083518625944,0.0779717130936404));
#5128=CARTESIAN_POINT('Ctrl Pts',(0.289136645896019,-2.71009877520201,0.08));
#5129=CARTESIAN_POINT('Ctrl Pts',(0.289136645896019,-2.7,0.08));
#5130=CARTESIAN_POINT('',(-0.3,-2.62,-3.65842984849668E-17));
#5131=CARTESIAN_POINT('Ctrl Pts',(-0.3,-2.62,-3.81639164714898E-17));
#5132=CARTESIAN_POINT('Ctrl Pts',(-0.3,-2.62,0.0100969318362555));
#5133=CARTESIAN_POINT('Ctrl Pts',(-0.299439403644655,-2.62202783742922,
0.0208340363410406));
#5134=CARTESIAN_POINT('Ctrl Pts',(-0.297414335384467,-2.63020753286176,
0.040530564260255));
#5135=CARTESIAN_POINT('Ctrl Pts',(-0.295976783522942,-2.63635675541778,
0.0494938404076283));
#5136=CARTESIAN_POINT('Ctrl Pts',(-0.293259762986909,-2.65050745119895,
0.0636445361887959));
#5137=CARTESIAN_POINT('Ctrl Pts',(-0.291799203044223,-2.65947019347274,
0.0697927537456147));
#5138=CARTESIAN_POINT('Ctrl Pts',(-0.289720927595908,-2.67916481374056,
0.0779717130936404));
#5139=CARTESIAN_POINT('Ctrl Pts',(-0.289136645896019,-2.68990122479799,
0.08));
#5140=CARTESIAN_POINT('Ctrl Pts',(-0.289136645896019,-2.7,0.08));
#5141=CARTESIAN_POINT('Ctrl Pts',(-0.3,-2.78,-6.93889390390723E-18));
#5142=CARTESIAN_POINT('Ctrl Pts',(-0.3,-2.78,-0.0100969318362556));
#5143=CARTESIAN_POINT('Ctrl Pts',(-0.299439403644655,-2.77797216257078,
-0.0208340363410406));
#5144=CARTESIAN_POINT('Ctrl Pts',(-0.297414335384467,-2.76979246713824,
-0.0405305642602551));
#5145=CARTESIAN_POINT('Ctrl Pts',(-0.295976783522942,-2.76364324458222,
-0.0494938404076283));
#5146=CARTESIAN_POINT('Ctrl Pts',(-0.293259762986909,-2.74949254880105,
-0.0636445361887959));
#5147=CARTESIAN_POINT('Ctrl Pts',(-0.291799203044223,-2.74052980652726,
-0.0697927537456147));
#5148=CARTESIAN_POINT('Ctrl Pts',(-0.289720927595908,-2.72083518625944,
-0.0779717130936403));
#5149=CARTESIAN_POINT('Ctrl Pts',(-0.289136645896019,-2.71009877520201,
-0.08));
#5150=CARTESIAN_POINT('Ctrl Pts',(-0.289136645896019,-2.68990122479799,
-0.08));
#5151=CARTESIAN_POINT('Ctrl Pts',(-0.289720927595908,-2.67916481374056,
-0.0779717130936403));
#5152=CARTESIAN_POINT('Ctrl Pts',(-0.291799203044223,-2.65947019347274,
-0.0697927537456147));
#5153=CARTESIAN_POINT('Ctrl Pts',(-0.293259762986909,-2.65050745119895,
-0.0636445361887959));
#5154=CARTESIAN_POINT('Ctrl Pts',(-0.295976783522942,-2.63635675541778,
-0.0494938404076283));
#5155=CARTESIAN_POINT('Ctrl Pts',(-0.297414335384467,-2.63020753286176,
-0.0405305642602551));
#5156=CARTESIAN_POINT('Ctrl Pts',(-0.299439403644655,-2.62202783742922,
-0.0208340363410406));
#5157=CARTESIAN_POINT('Ctrl Pts',(-0.3,-2.62,-0.0100969318362556));
#5158=CARTESIAN_POINT('Ctrl Pts',(-0.3,-2.62,-1.56125112837913E-17));
#5159=CARTESIAN_POINT('Origin',(0.45,0.2,0.));
#5160=CARTESIAN_POINT('',(-0.45,0.2,-5.51091059616309E-17));
#5161=CARTESIAN_POINT('Origin',(0.,0.2,0.));
#5162=CARTESIAN_POINT('Origin',(0.,0.175,0.));
#5163=CARTESIAN_POINT('',(-0.5,0.15,-6.12323399573676E-17));
#5164=CARTESIAN_POINT('Origin',(0.,0.15,0.));
#5165=CARTESIAN_POINT('',(-0.475,0.175,-5.81707229594993E-17));
#5166=CARTESIAN_POINT('Origin',(0.,0.0750000000000002,0.));
#5167=CARTESIAN_POINT('',(-0.5,0.,-6.12323399573677E-17));
#5168=CARTESIAN_POINT('Origin',(0.,0.,0.));
#5169=CARTESIAN_POINT('',(-0.5,0.0750000000000002,-6.12323399573677E-17));
#5170=CARTESIAN_POINT('Origin',(0.3,0.,0.));
#5171=CARTESIAN_POINT('',(-0.3,0.,-3.67394039744206E-17));
#5172=CARTESIAN_POINT('Origin',(0.,0.,0.));
#5173=CARTESIAN_POINT('Origin',(0.,-1.455,0.));
#5174=CARTESIAN_POINT('',(-0.3,-2.91,-3.67394039744206E-17));
#5175=CARTESIAN_POINT('Origin',(0.,-2.91,0.));
#5176=CARTESIAN_POINT('',(-0.3,-1.455,-3.67394039744206E-17));
#5177=CARTESIAN_POINT('',(-0.3,-1.455,-3.67394039744206E-17));
#5178=CARTESIAN_POINT('Origin',(0.,-2.955,0.));
#5179=CARTESIAN_POINT('',(-0.21,-3.,-2.57175827820944E-17));
#5180=CARTESIAN_POINT('Origin',(0.,-3.,0.));
#5181=CARTESIAN_POINT('',(-0.255,-2.955,-3.12284933782575E-17));
#5182=CARTESIAN_POINT('Origin',(0.,-3.,0.));
#5183=CARTESIAN_POINT('',(0.,0.,0.));
#5184=CARTESIAN_POINT('Origin',(0.,0.,0.));
#5185=CARTESIAN_POINT('',(-0.32,0.16,3.91886975727153E-17));
#5186=CARTESIAN_POINT('Origin',(0.,0.16,0.));
#5187=CARTESIAN_POINT('',(-0.32,0.,3.91886975727153E-17));
#5188=CARTESIAN_POINT('',(-0.32,0.,3.91886975727153E-17));
#5189=CARTESIAN_POINT('Origin',(0.,0.,0.));
#5190=CARTESIAN_POINT('Origin',(0.,0.,0.));
#5191=CARTESIAN_POINT('',(-0.6,0.16,7.34788079488412E-17));
#5192=CARTESIAN_POINT('Origin',(0.,0.16,0.));
#5193=CARTESIAN_POINT('',(-0.6,0.,7.34788079488412E-17));
#5194=CARTESIAN_POINT('',(-0.6,0.,7.34788079488412E-17));
#5195=CARTESIAN_POINT('Origin',(0.,0.,0.));
#5196=CARTESIAN_POINT('Origin',(0.,0.16,0.));
#5197=CARTESIAN_POINT('Origin',(0.,0.,0.));
#5198=CARTESIAN_POINT('',(0.,0.,0.));
#5199=CARTESIAN_POINT('',(0.,-1.06,2.5));
#5200=CARTESIAN_POINT('',(0.,-1.06,2.5));
#5201=CARTESIAN_POINT('',(0.,0.,0.));
#5202=CARTESIAN_POINT('',(0.,0.,0.));
#5203=CARTESIAN_POINT('Origin',(0.,0.12,0.));
#5204=CARTESIAN_POINT('',(-9.79717439317883E-18,0.12,-0.04));
#5205=CARTESIAN_POINT('Origin',(0.,0.12,-0.12));
#5206=CARTESIAN_POINT('Origin',(9.79717439317883E-18,0.12,0.));
#5207=CARTESIAN_POINT('',(0.08,-4.89858719658941E-18,7.34788079488412E-18));
#5208=CARTESIAN_POINT('',(-0.08,-4.89858719658941E-18,7.34788079488412E-18));
#5209=CARTESIAN_POINT('Ctrl Pts',(0.08,-4.89858719658941E-18,7.34788079488412E-18));
#5210=CARTESIAN_POINT('Ctrl Pts',(0.08,-0.00012864962353541,0.000128649623535413));
#5211=CARTESIAN_POINT('Ctrl Pts',(0.0799996896739287,-0.00025719571182076,
0.000257402596003253));
#5212=CARTESIAN_POINT('Ctrl Pts',(0.0799669711262291,-0.00701193164572964,
0.00703384588894362));
#5213=CARTESIAN_POINT('Ctrl Pts',(0.0791054994909294,-0.0133457972655825,
0.0139383126556792));
#5214=CARTESIAN_POINT('Ctrl Pts',(0.0749700088488058,-0.0265076530862524,
0.0292212026164895));
#5215=CARTESIAN_POINT('Ctrl Pts',(0.0712702072865517,-0.0331317062461458,
0.0375603420117568));
#5216=CARTESIAN_POINT('Ctrl Pts',(0.0612858949407667,-0.0440683985740427,
0.0520545604187517));
#5217=CARTESIAN_POINT('Ctrl Pts',(0.0555090276731744,-0.0485199197794574,
0.0582717815295611));
#5218=CARTESIAN_POINT('Ctrl Pts',(0.0412398082144208,-0.0561090538733877,
0.0691638397919718));
#5219=CARTESIAN_POINT('Ctrl Pts',(0.0327878980890048,-0.059089642483296,
0.0736229049587921));
#5220=CARTESIAN_POINT('Ctrl Pts',(0.0159233027310102,-0.0625179833270725,
0.0787936360751706));
#5221=CARTESIAN_POINT('Ctrl Pts',(0.00801661414593076,-0.0633030277982336,
0.08));
#5222=CARTESIAN_POINT('Ctrl Pts',(-0.00801661414593074,-0.0633030277982336,
0.08));
#5223=CARTESIAN_POINT('Ctrl Pts',(-0.0159233027310102,-0.0625179833270726,
0.0787936360751706));
#5224=CARTESIAN_POINT('Ctrl Pts',(-0.0327878980890049,-0.059089642483296,
0.0736229049587921));
#5225=CARTESIAN_POINT('Ctrl Pts',(-0.0412398082144209,-0.0561090538733877,
0.0691638397919717));
#5226=CARTESIAN_POINT('Ctrl Pts',(-0.0555090276731744,-0.0485199197794574,
0.0582717815295611));
#5227=CARTESIAN_POINT('Ctrl Pts',(-0.0612858949407667,-0.0440683985740427,
0.0520545604187517));
#5228=CARTESIAN_POINT('Ctrl Pts',(-0.0712702072865517,-0.0331317062461458,
0.0375603420117568));
#5229=CARTESIAN_POINT('Ctrl Pts',(-0.0749700088488058,-0.0265076530862524,
0.0292212026164895));
#5230=CARTESIAN_POINT('Ctrl Pts',(-0.0791054994909264,-0.0133457972655921,
0.0139383126556903));
#5231=CARTESIAN_POINT('Ctrl Pts',(-0.0799669711262287,-0.00701193164579759,
0.0070338458890125));
#5232=CARTESIAN_POINT('Ctrl Pts',(-0.0799996896739287,-0.000257195711817665,
0.000257402596000083));
#5233=CARTESIAN_POINT('Ctrl Pts',(-0.08,-0.000128649623538514,0.000128649623538516));
#5234=CARTESIAN_POINT('Ctrl Pts',(-0.08,-4.89858719658941E-18,7.34788079488412E-18));
#5235=CARTESIAN_POINT('Ctrl Pts',(-0.08,-4.89858719658941E-18,7.34788079488412E-18));
#5236=CARTESIAN_POINT('Ctrl Pts',(-0.08,-0.000128649623536042,-0.00012864962353603));
#5237=CARTESIAN_POINT('Ctrl Pts',(-0.0799996896739287,-0.000257195711820127,
-0.000257402596002604));
#5238=CARTESIAN_POINT('Ctrl Pts',(-0.0799669711262289,-0.0070119316457589,
-0.00703384588897312));
#5239=CARTESIAN_POINT('Ctrl Pts',(-0.0791054994909281,-0.0133457972655867,
-0.0139383126556841));
#5240=CARTESIAN_POINT('Ctrl Pts',(-0.0749700088488058,-0.0265076530862525,
-0.0292212026164896));
#5241=CARTESIAN_POINT('Ctrl Pts',(-0.0712702072865516,-0.0331317062461459,
-0.0375603420117568));
#5242=CARTESIAN_POINT('Ctrl Pts',(-0.0612858949407667,-0.0440683985740427,
-0.0520545604187517));
#5243=CARTESIAN_POINT('Ctrl Pts',(-0.0555090276731744,-0.0485199197794574,
-0.0582717815295611));
#5244=CARTESIAN_POINT('Ctrl Pts',(-0.0412398082144209,-0.0561090538733877,
-0.0691638397919717));
#5245=CARTESIAN_POINT('Ctrl Pts',(-0.0327878980890049,-0.059089642483296,
-0.0736229049587921));
#5246=CARTESIAN_POINT('Ctrl Pts',(-0.0159233027310101,-0.0625179833270725,
-0.0787936360751706));
#5247=CARTESIAN_POINT('Ctrl Pts',(-0.00801661414593069,-0.0633030277982336,
-0.08));
#5248=CARTESIAN_POINT('Ctrl Pts',(0.0080166141459307,-0.0633030277982336,
-0.08));
#5249=CARTESIAN_POINT('Ctrl Pts',(0.0159233027310101,-0.0625179833270725,
-0.0787936360751706));
#5250=CARTESIAN_POINT('Ctrl Pts',(0.0327878980890049,-0.0590896424832959,
-0.0736229049587921));
#5251=CARTESIAN_POINT('Ctrl Pts',(0.0412398082144209,-0.0561090538733877,
-0.0691638397919717));
#5252=CARTESIAN_POINT('Ctrl Pts',(0.0555090276731744,-0.0485199197794574,
-0.0582717815295611));
#5253=CARTESIAN_POINT('Ctrl Pts',(0.0612858949407666,-0.0440683985740428,
-0.0520545604187518));
#5254=CARTESIAN_POINT('Ctrl Pts',(0.0712702072865517,-0.0331317062461458,
-0.0375603420117568));
#5255=CARTESIAN_POINT('Ctrl Pts',(0.0749700088488058,-0.0265076530862524,
-0.0292212026164895));
#5256=CARTESIAN_POINT('Ctrl Pts',(0.079105499490928,-0.013345797265587,
-0.0139383126556845));
#5257=CARTESIAN_POINT('Ctrl Pts',(0.0799669711262289,-0.00701193164576148,
-0.00703384588897579));
#5258=CARTESIAN_POINT('Ctrl Pts',(0.0799996896739287,-0.000257195711819584,
-0.000257402596002039));
#5259=CARTESIAN_POINT('Ctrl Pts',(0.08,-0.000128649623536605,-0.000128649623536593));
#5260=CARTESIAN_POINT('Ctrl Pts',(0.08,-4.89858719658941E-18,7.34788079488412E-18));
#5261=CARTESIAN_POINT('Origin',(0.04,-1.36,0.));
#5262=CARTESIAN_POINT('',(0.,-1.36,-0.08));
#5263=CARTESIAN_POINT('',(0.,-1.36,0.08));
#5264=CARTESIAN_POINT('Origin',(0.,-1.36,0.));
#5265=CARTESIAN_POINT('',(0.,-1.36,-0.04));
#5266=CARTESIAN_POINT('Origin',(0.,0.,-0.08));
#5267=CARTESIAN_POINT('',(0.,-1.6,0.08));
#5268=CARTESIAN_POINT('',(0.,0.,0.08));
#5269=CARTESIAN_POINT('',(0.,-1.6,-0.08));
#5270=CARTESIAN_POINT('',(0.,-1.6,-0.09));
#5271=CARTESIAN_POINT('',(0.,0.,-0.08));
#5272=CARTESIAN_POINT('Origin',(0.,0.,0.));
#5273=CARTESIAN_POINT('',(-0.08,-1.6,-9.79717439317883E-18));
#5274=CARTESIAN_POINT('Origin',(0.,-1.6,0.));
#5275=CARTESIAN_POINT('',(-0.08,0.,-9.79717439317883E-18));
#5276=CARTESIAN_POINT('Origin',(0.,-1.6,0.));
#5277=CARTESIAN_POINT('Origin',(-0.04,-1.6,0.));
#5278=CARTESIAN_POINT('',(0.,0.,0.));
#5279=CARTESIAN_POINT('',(0.,0.,0.));
#5280=CARTESIAN_POINT('',(0.,0.,0.));
#5281=CARTESIAN_POINT('',(-5.97716818855047,6.1,-8.05293445648595));
#5282=CARTESIAN_POINT('',(-5.97716818855047,0.4,1.97706554351405));
#5283=CARTESIAN_POINT('',(-2.49048674522936,1.86,2.28211064313086));
#5284=CARTESIAN_POINT('',(-2.49048674522936,-0.56,2.28211064313086));
#5285=CARTESIAN_POINT('',(-2.49048674522936,1.7,2.28211064313086));
#5286=CARTESIAN_POINT('',(-2.89048674522936,-0.84,2.28211064313086));
#5287=CARTESIAN_POINT('',(0.,0.,0.));
#5288=CARTESIAN_POINT('Origin',(15.,0.,4.5));
#5289=CARTESIAN_POINT('',(14.5,-0.4,4.5));
#5290=CARTESIAN_POINT('Origin',(14.5,0.,4.5));
#5291=CARTESIAN_POINT('',(15.,-0.4,4.5));
#5292=CARTESIAN_POINT('',(15.,-0.4,4.5));
#5293=CARTESIAN_POINT('',(15.,4.89858719658941E-17,4.1));
#5294=CARTESIAN_POINT('Origin',(15.,0.,4.5));
#5295=CARTESIAN_POINT('Origin',(15.,0.,4.5));
#5296=CARTESIAN_POINT('Origin',(15.,0.,3.5));
#5297=CARTESIAN_POINT('',(15.,4.89858719658941E-17,2.9));
#5298=CARTESIAN_POINT('Origin',(15.,4.89858719658941E-17,3.5));
#5299=CARTESIAN_POINT('',(15.,-0.4,2.5));
#5300=CARTESIAN_POINT('Origin',(15.,0.,2.5));
#5301=CARTESIAN_POINT('Origin',(15.,0.,2.5));
#5302=CARTESIAN_POINT('Origin',(10.,0.,2.5));
#5303=CARTESIAN_POINT('',(10.,-0.4,2.5));
#5304=CARTESIAN_POINT('',(10.,-0.4,2.5));
#5305=CARTESIAN_POINT('Origin',(10.,0.,2.5));
#5306=CARTESIAN_POINT('Origin',(14.5,0.,4.5));
#5307=CARTESIAN_POINT('Origin',(10.,0.,2.5));
#5308=CARTESIAN_POINT('',(0.,0.,0.));
#5309=CARTESIAN_POINT('Origin',(0.,0.,0.));
#5310=CARTESIAN_POINT('',(-0.42,0.16,5.14351655641888E-17));
#5311=CARTESIAN_POINT('Origin',(0.,0.16,0.));
#5312=CARTESIAN_POINT('',(-0.42,0.,5.14351655641888E-17));
#5313=CARTESIAN_POINT('',(-0.42,0.,5.14351655641888E-17));
#5314=CARTESIAN_POINT('Origin',(0.,0.,0.));
#5315=CARTESIAN_POINT('Origin',(0.,0.,0.));
#5316=CARTESIAN_POINT('',(-0.8,0.16,9.79717439317883E-17));
#5317=CARTESIAN_POINT('Origin',(0.,0.16,0.));
#5318=CARTESIAN_POINT('',(-0.8,0.,9.79717439317883E-17));
#5319=CARTESIAN_POINT('',(-0.8,0.,9.79717439317883E-17));
#5320=CARTESIAN_POINT('Origin',(0.,0.,0.));
#5321=CARTESIAN_POINT('Origin',(0.,0.16,0.));
#5322=CARTESIAN_POINT('Origin',(0.,0.,0.));
#5323=CARTESIAN_POINT('',(0.,0.,0.));
#5324=CARTESIAN_POINT('Origin',(0.,0.067277284513851,0.));
#5325=CARTESIAN_POINT('',(-0.375277674973257,0.0768195421087395,0.65));
#5326=CARTESIAN_POINT('',(0.375277674973257,0.0768195421087395,0.65));
#5327=CARTESIAN_POINT('Ctrl Pts',(-0.375277674973257,0.0768195421087395,
0.65));
#5328=CARTESIAN_POINT('Ctrl Pts',(1.66533453693773E-13,-0.0315137912242439,
0.65));
#5329=CARTESIAN_POINT('Ctrl Pts',(0.375277674973257,0.0768195421087394,
0.65));
#5330=CARTESIAN_POINT('',(-0.750555349946514,0.0768195421087394,-9.19165206894919E-17));
#5331=CARTESIAN_POINT('Ctrl Pts',(-0.750555349946514,0.0768195421087394,
-9.19165206894919E-17));
#5332=CARTESIAN_POINT('Ctrl Pts',(-0.562916512459802,-0.0315137912242434,
0.325000000000144));
#5333=CARTESIAN_POINT('Ctrl Pts',(-0.375277674973257,0.0768195421087395,
0.65));
#5334=CARTESIAN_POINT('',(-0.6175,-2.77555756156289E-17,-7.5621939847349E-17));
#5335=CARTESIAN_POINT('',(-0.734027674973257,0.067277284513851,-8.98924642641573E-17));
#5336=CARTESIAN_POINT('Origin',(0.,0.,0.));
#5337=CARTESIAN_POINT('',(-0.375277674973257,0.0768195421087395,-0.65));
#5338=CARTESIAN_POINT('Ctrl Pts',(-0.375277674973257,0.0768195421087395,
-0.65));
#5339=CARTESIAN_POINT('Ctrl Pts',(-0.562916512459968,-0.0315137912242437,
-0.324999999999856));
#5340=CARTESIAN_POINT('Ctrl Pts',(-0.750555349946514,0.0768195421087395,
-9.19165206894919E-17));
#5341=CARTESIAN_POINT('',(0.375277674973257,0.0768195421087395,-0.65));
#5342=CARTESIAN_POINT('Ctrl Pts',(0.375277674973257,0.0768195421087395,
-0.65));
#5343=CARTESIAN_POINT('Ctrl Pts',(-1.66144875635155E-13,-0.0315137912242437,
-0.65));
#5344=CARTESIAN_POINT('Ctrl Pts',(-0.375277674973257,0.0768195421087395,
-0.65));
#5345=CARTESIAN_POINT('',(0.750555349946514,0.0768195421087394,0.));
#5346=CARTESIAN_POINT('Ctrl Pts',(0.750555349946514,0.0768195421087394,
0.));
#5347=CARTESIAN_POINT('Ctrl Pts',(0.562916512459802,-0.0315137912242436,
-0.325000000000144));
#5348=CARTESIAN_POINT('Ctrl Pts',(0.375277674973257,0.0768195421087395,
-0.65));
#5349=CARTESIAN_POINT('Ctrl Pts',(0.375277674973257,0.0768195421087394,
0.65));
#5350=CARTESIAN_POINT('Ctrl Pts',(0.562916512459968,-0.0315137912242439,
0.324999999999856));
#5351=CARTESIAN_POINT('Ctrl Pts',(0.750555349946514,0.0768195421087394,
0.));
#5352=CARTESIAN_POINT('Origin',(0.,0.612722715486149,0.));
#5353=CARTESIAN_POINT('',(-0.6175,0.68,-7.5621939847349E-17));
#5354=CARTESIAN_POINT('Origin',(0.,0.68,0.));
#5355=CARTESIAN_POINT('',(-0.750555349946514,0.603180457891261,-9.19165206894919E-17));
#5356=CARTESIAN_POINT('',(-0.734027674973257,0.612722715486149,-8.98924642641573E-17));
#5357=CARTESIAN_POINT('',(-0.375277674973257,0.603180457891261,0.65));
#5358=CARTESIAN_POINT('Ctrl Pts',(-0.375277674973257,0.603180457891261,
0.65));
#5359=CARTESIAN_POINT('Ctrl Pts',(-0.562916512459968,0.711513791224243,
0.324999999999856));
#5360=CARTESIAN_POINT('Ctrl Pts',(-0.750555349946514,0.603180457891261,
-9.19165206894919E-17));
#5361=CARTESIAN_POINT('',(0.375277674973257,0.603180457891261,0.65));
#5362=CARTESIAN_POINT('Ctrl Pts',(0.375277674973257,0.603180457891261,0.65));
#5363=CARTESIAN_POINT('Ctrl Pts',(-1.66755498298699E-13,0.711513791224244,
0.65));
#5364=CARTESIAN_POINT('Ctrl Pts',(-0.375277674973257,0.603180457891261,
0.65));
#5365=CARTESIAN_POINT('',(0.750555349946514,0.603180457891261,0.));
#5366=CARTESIAN_POINT('Ctrl Pts',(0.750555349946514,0.603180457891261,0.));
#5367=CARTESIAN_POINT('Ctrl Pts',(0.562916512459802,0.711513791224244,0.325000000000144));
#5368=CARTESIAN_POINT('Ctrl Pts',(0.375277674973257,0.603180457891261,0.65));
#5369=CARTESIAN_POINT('',(0.375277674973257,0.603180457891261,-0.65));
#5370=CARTESIAN_POINT('Ctrl Pts',(0.375277674973257,0.603180457891261,-0.65));
#5371=CARTESIAN_POINT('Ctrl Pts',(0.562916512459969,0.711513791224244,-0.324999999999856));
#5372=CARTESIAN_POINT('Ctrl Pts',(0.750555349946514,0.603180457891261,0.));
#5373=CARTESIAN_POINT('',(-0.375277674973257,0.603180457891261,-0.65));
#5374=CARTESIAN_POINT('Ctrl Pts',(-0.375277674973257,0.603180457891261,
-0.65));
#5375=CARTESIAN_POINT('Ctrl Pts',(1.66422431391311E-13,0.711513791224244,
-0.65));
#5376=CARTESIAN_POINT('Ctrl Pts',(0.375277674973257,0.603180457891261,-0.65));
#5377=CARTESIAN_POINT('Ctrl Pts',(-0.750555349946514,0.603180457891261,
-9.19165206894919E-17));
#5378=CARTESIAN_POINT('Ctrl Pts',(-0.562916512459802,0.711513791224244,
-0.325000000000144));
#5379=CARTESIAN_POINT('Ctrl Pts',(-0.375277674973257,0.603180457891261,
-0.65));
#5380=CARTESIAN_POINT('Origin',(0.375277674973257,0.,-0.65));
#5381=CARTESIAN_POINT('',(-0.375277674973257,0.,-0.65));
#5382=CARTESIAN_POINT('',(0.375277674973257,0.,-0.65));
#5383=CARTESIAN_POINT('Origin',(-0.375277674973257,0.,-0.65));
#5384=CARTESIAN_POINT('',(-0.750555349946514,0.,-9.19165206894919E-17));
#5385=CARTESIAN_POINT('Origin',(-0.750555349946514,0.,-9.19165206894919E-17));
#5386=CARTESIAN_POINT('',(-0.375277674973257,0.,0.65));
#5387=CARTESIAN_POINT('Origin',(0.,0.,0.));
#5388=CARTESIAN_POINT('',(-0.338975,0.68,4.15124648740974E-17));
#5389=CARTESIAN_POINT('Origin',(0.,0.68,0.));
#5390=CARTESIAN_POINT('',(-0.338975,0.,4.15124648740974E-17));
#5391=CARTESIAN_POINT('',(-0.338975,0.,4.15124648740974E-17));
#5392=CARTESIAN_POINT('Origin',(0.,0.,0.));
#5393=CARTESIAN_POINT('Origin',(-0.375277674973257,0.,0.65));
#5394=CARTESIAN_POINT('',(0.375277674973257,0.,0.65));
#5395=CARTESIAN_POINT('Origin',(0.750555349946514,0.,0.));
#5396=CARTESIAN_POINT('',(0.750555349946514,0.,0.));
#5397=CARTESIAN_POINT('Origin',(0.375277674973257,0.,0.65));
#5398=CARTESIAN_POINT('Origin',(0.,0.68,-1.11022302462516E-16));
#5399=CARTESIAN_POINT('Origin',(0.,0.,-1.11022302462516E-16));
#5400=CARTESIAN_POINT('',(0.,0.,0.));
#5401=CARTESIAN_POINT('',(0.,0.,0.));
#5402=CARTESIAN_POINT('',(2.00423507354465,2.28,2.5));
#5403=CARTESIAN_POINT('',(2.00423507354465,0.94,2.5));
#5404=CARTESIAN_POINT('',(2.00423507354465,2.12,2.5));
#5405=CARTESIAN_POINT('',(1.60423507354465,-0.42,2.5));
#5406=CARTESIAN_POINT('',(0.,0.,0.));
#5407=CARTESIAN_POINT('',(11.,0.,2.5));
#5408=CARTESIAN_POINT('',(11.16,0.,2.5));
#5409=CARTESIAN_POINT('',(0.,0.,0.));
#5410=CARTESIAN_POINT('',(0.,0.,0.));
#5411=CARTESIAN_POINT('',(0.,0.,0.));
#5412=CARTESIAN_POINT('',(0.,0.,0.));
#5413=UNCERTAINTY_MEASURE_WITH_UNIT(LENGTH_MEASURE(0.001),#5459,
'DISTANCE_ACCURACY_VALUE',
'Maximum model space distance between geometric entities at asserted c
onnectivities');
#5414=UNCERTAINTY_MEASURE_WITH_UNIT(LENGTH_MEASURE(0.001),#5459,
'DISTANCE_ACCURACY_VALUE',
'Maximum model space distance between geometric entities at asserted c
onnectivities');
#5415=UNCERTAINTY_MEASURE_WITH_UNIT(LENGTH_MEASURE(0.001),#5459,
'DISTANCE_ACCURACY_VALUE',
'Maximum model space distance between geometric entities at asserted c
onnectivities');
#5416=UNCERTAINTY_MEASURE_WITH_UNIT(LENGTH_MEASURE(0.001),#5459,
'DISTANCE_ACCURACY_VALUE',
'Maximum model space distance between geometric entities at asserted c
onnectivities');
#5417=UNCERTAINTY_MEASURE_WITH_UNIT(LENGTH_MEASURE(0.001),#5459,
'DISTANCE_ACCURACY_VALUE',
'Maximum model space distance between geometric entities at asserted c
onnectivities');
#5418=UNCERTAINTY_MEASURE_WITH_UNIT(LENGTH_MEASURE(0.001),#5459,
'DISTANCE_ACCURACY_VALUE',
'Maximum model space distance between geometric entities at asserted c
onnectivities');
#5419=UNCERTAINTY_MEASURE_WITH_UNIT(LENGTH_MEASURE(0.001),#5459,
'DISTANCE_ACCURACY_VALUE',
'Maximum model space distance between geometric entities at asserted c
onnectivities');
#5420=UNCERTAINTY_MEASURE_WITH_UNIT(LENGTH_MEASURE(0.001),#5459,
'DISTANCE_ACCURACY_VALUE',
'Maximum model space distance between geometric entities at asserted c
onnectivities');
#5421=UNCERTAINTY_MEASURE_WITH_UNIT(LENGTH_MEASURE(0.001),#5459,
'DISTANCE_ACCURACY_VALUE',
'Maximum model space distance between geometric entities at asserted c
onnectivities');
#5422=UNCERTAINTY_MEASURE_WITH_UNIT(LENGTH_MEASURE(0.001),#5459,
'DISTANCE_ACCURACY_VALUE',
'Maximum model space distance between geometric entities at asserted c
onnectivities');
#5423=UNCERTAINTY_MEASURE_WITH_UNIT(LENGTH_MEASURE(0.001),#5459,
'DISTANCE_ACCURACY_VALUE',
'Maximum model space distance between geometric entities at asserted c
onnectivities');
#5424=UNCERTAINTY_MEASURE_WITH_UNIT(LENGTH_MEASURE(0.001),#5459,
'DISTANCE_ACCURACY_VALUE',
'Maximum model space distance between geometric entities at asserted c
onnectivities');
#5425=UNCERTAINTY_MEASURE_WITH_UNIT(LENGTH_MEASURE(0.001),#5459,
'DISTANCE_ACCURACY_VALUE',
'Maximum model space distance between geometric entities at asserted c
onnectivities');
#5426=UNCERTAINTY_MEASURE_WITH_UNIT(LENGTH_MEASURE(0.001),#5459,
'DISTANCE_ACCURACY_VALUE',
'Maximum model space distance between geometric entities at asserted c
onnectivities');
#5427=UNCERTAINTY_MEASURE_WITH_UNIT(LENGTH_MEASURE(0.001),#5459,
'DISTANCE_ACCURACY_VALUE',
'Maximum model space distance between geometric entities at asserted c
onnectivities');
#5428=UNCERTAINTY_MEASURE_WITH_UNIT(LENGTH_MEASURE(0.001),#5459,
'DISTANCE_ACCURACY_VALUE',
'Maximum model space distance between geometric entities at asserted c
onnectivities');
#5429=UNCERTAINTY_MEASURE_WITH_UNIT(LENGTH_MEASURE(0.001),#5459,
'DISTANCE_ACCURACY_VALUE',
'Maximum model space distance between geometric entities at asserted c
onnectivities');
#5430=UNCERTAINTY_MEASURE_WITH_UNIT(LENGTH_MEASURE(0.001),#5459,
'DISTANCE_ACCURACY_VALUE',
'Maximum model space distance between geometric entities at asserted c
onnectivities');
#5431=UNCERTAINTY_MEASURE_WITH_UNIT(LENGTH_MEASURE(0.001),#5459,
'DISTANCE_ACCURACY_VALUE',
'Maximum model space distance between geometric entities at asserted c
onnectivities');
#5432=UNCERTAINTY_MEASURE_WITH_UNIT(LENGTH_MEASURE(0.001),#5459,
'DISTANCE_ACCURACY_VALUE',
'Maximum model space distance between geometric entities at asserted c
onnectivities');
#5433=UNCERTAINTY_MEASURE_WITH_UNIT(LENGTH_MEASURE(0.001),#5459,
'DISTANCE_ACCURACY_VALUE',
'Maximum model space distance between geometric entities at asserted c
onnectivities');
#5434=UNCERTAINTY_MEASURE_WITH_UNIT(LENGTH_MEASURE(0.001),#5459,
'DISTANCE_ACCURACY_VALUE',
'Maximum model space distance between geometric entities at asserted c
onnectivities');
#5435=UNCERTAINTY_MEASURE_WITH_UNIT(LENGTH_MEASURE(0.001),#5459,
'DISTANCE_ACCURACY_VALUE',
'Maximum model space distance between geometric entities at asserted c
onnectivities');
#5436=(
GEOMETRIC_REPRESENTATION_CONTEXT(3)
GLOBAL_UNCERTAINTY_ASSIGNED_CONTEXT((#5413))
GLOBAL_UNIT_ASSIGNED_CONTEXT((#5459,#5461,#5462))
REPRESENTATION_CONTEXT('','3D')
);
#5437=(
GEOMETRIC_REPRESENTATION_CONTEXT(3)
GLOBAL_UNCERTAINTY_ASSIGNED_CONTEXT((#5414))
GLOBAL_UNIT_ASSIGNED_CONTEXT((#5459,#5461,#5462))
REPRESENTATION_CONTEXT('','3D')
);
#5438=(
GEOMETRIC_REPRESENTATION_CONTEXT(3)
GLOBAL_UNCERTAINTY_ASSIGNED_CONTEXT((#5415))
GLOBAL_UNIT_ASSIGNED_CONTEXT((#5459,#5461,#5462))
REPRESENTATION_CONTEXT('','3D')
);
#5439=(
GEOMETRIC_REPRESENTATION_CONTEXT(3)
GLOBAL_UNCERTAINTY_ASSIGNED_CONTEXT((#5416))
GLOBAL_UNIT_ASSIGNED_CONTEXT((#5459,#5461,#5462))
REPRESENTATION_CONTEXT('','3D')
);
#5440=(
GEOMETRIC_REPRESENTATION_CONTEXT(3)
GLOBAL_UNCERTAINTY_ASSIGNED_CONTEXT((#5417))
GLOBAL_UNIT_ASSIGNED_CONTEXT((#5459,#5461,#5462))
REPRESENTATION_CONTEXT('','3D')
);
#5441=(
GEOMETRIC_REPRESENTATION_CONTEXT(3)
GLOBAL_UNCERTAINTY_ASSIGNED_CONTEXT((#5418))
GLOBAL_UNIT_ASSIGNED_CONTEXT((#5459,#5461,#5462))
REPRESENTATION_CONTEXT('','3D')
);
#5442=(
GEOMETRIC_REPRESENTATION_CONTEXT(3)
GLOBAL_UNCERTAINTY_ASSIGNED_CONTEXT((#5419))
GLOBAL_UNIT_ASSIGNED_CONTEXT((#5459,#5461,#5462))
REPRESENTATION_CONTEXT('','3D')
);
#5443=(
GEOMETRIC_REPRESENTATION_CONTEXT(3)
GLOBAL_UNCERTAINTY_ASSIGNED_CONTEXT((#5420))
GLOBAL_UNIT_ASSIGNED_CONTEXT((#5459,#5461,#5462))
REPRESENTATION_CONTEXT('','3D')
);
#5444=(
GEOMETRIC_REPRESENTATION_CONTEXT(3)
GLOBAL_UNCERTAINTY_ASSIGNED_CONTEXT((#5421))
GLOBAL_UNIT_ASSIGNED_CONTEXT((#5459,#5461,#5462))
REPRESENTATION_CONTEXT('','3D')
);
#5445=(
GEOMETRIC_REPRESENTATION_CONTEXT(3)
GLOBAL_UNCERTAINTY_ASSIGNED_CONTEXT((#5422))
GLOBAL_UNIT_ASSIGNED_CONTEXT((#5459,#5461,#5462))
REPRESENTATION_CONTEXT('','3D')
);
#5446=(
GEOMETRIC_REPRESENTATION_CONTEXT(3)
GLOBAL_UNCERTAINTY_ASSIGNED_CONTEXT((#5423))
GLOBAL_UNIT_ASSIGNED_CONTEXT((#5459,#5461,#5462))
REPRESENTATION_CONTEXT('','3D')
);
#5447=(
GEOMETRIC_REPRESENTATION_CONTEXT(3)
GLOBAL_UNCERTAINTY_ASSIGNED_CONTEXT((#5424))
GLOBAL_UNIT_ASSIGNED_CONTEXT((#5459,#5461,#5462))
REPRESENTATION_CONTEXT('','3D')
);
#5448=(
GEOMETRIC_REPRESENTATION_CONTEXT(3)
GLOBAL_UNCERTAINTY_ASSIGNED_CONTEXT((#5425))
GLOBAL_UNIT_ASSIGNED_CONTEXT((#5459,#5461,#5462))
REPRESENTATION_CONTEXT('','3D')
);
#5449=(
GEOMETRIC_REPRESENTATION_CONTEXT(3)
GLOBAL_UNCERTAINTY_ASSIGNED_CONTEXT((#5426))
GLOBAL_UNIT_ASSIGNED_CONTEXT((#5459,#5461,#5462))
REPRESENTATION_CONTEXT('','3D')
);
#5450=(
GEOMETRIC_REPRESENTATION_CONTEXT(3)
GLOBAL_UNCERTAINTY_ASSIGNED_CONTEXT((#5427))
GLOBAL_UNIT_ASSIGNED_CONTEXT((#5459,#5461,#5462))
REPRESENTATION_CONTEXT('','3D')
);
#5451=(
GEOMETRIC_REPRESENTATION_CONTEXT(3)
GLOBAL_UNCERTAINTY_ASSIGNED_CONTEXT((#5428))
GLOBAL_UNIT_ASSIGNED_CONTEXT((#5459,#5461,#5462))
REPRESENTATION_CONTEXT('','3D')
);
#5452=(
GEOMETRIC_REPRESENTATION_CONTEXT(3)
GLOBAL_UNCERTAINTY_ASSIGNED_CONTEXT((#5429))
GLOBAL_UNIT_ASSIGNED_CONTEXT((#5459,#5461,#5462))
REPRESENTATION_CONTEXT('','3D')
);
#5453=(
GEOMETRIC_REPRESENTATION_CONTEXT(3)
GLOBAL_UNCERTAINTY_ASSIGNED_CONTEXT((#5430))
GLOBAL_UNIT_ASSIGNED_CONTEXT((#5459,#5461,#5462))
REPRESENTATION_CONTEXT('','3D')
);
#5454=(
GEOMETRIC_REPRESENTATION_CONTEXT(3)
GLOBAL_UNCERTAINTY_ASSIGNED_CONTEXT((#5431))
GLOBAL_UNIT_ASSIGNED_CONTEXT((#5459,#5461,#5462))
REPRESENTATION_CONTEXT('','3D')
);
#5455=(
GEOMETRIC_REPRESENTATION_CONTEXT(3)
GLOBAL_UNCERTAINTY_ASSIGNED_CONTEXT((#5432))
GLOBAL_UNIT_ASSIGNED_CONTEXT((#5459,#5461,#5462))
REPRESENTATION_CONTEXT('','3D')
);
#5456=(
GEOMETRIC_REPRESENTATION_CONTEXT(3)
GLOBAL_UNCERTAINTY_ASSIGNED_CONTEXT((#5433))
GLOBAL_UNIT_ASSIGNED_CONTEXT((#5459,#5461,#5462))
REPRESENTATION_CONTEXT('','3D')
);
#5457=(
GEOMETRIC_REPRESENTATION_CONTEXT(3)
GLOBAL_UNCERTAINTY_ASSIGNED_CONTEXT((#5434))
GLOBAL_UNIT_ASSIGNED_CONTEXT((#5459,#5461,#5462))
REPRESENTATION_CONTEXT('','3D')
);
#5458=(
GEOMETRIC_REPRESENTATION_CONTEXT(3)
GLOBAL_UNCERTAINTY_ASSIGNED_CONTEXT((#5435))
GLOBAL_UNIT_ASSIGNED_CONTEXT((#5459,#5461,#5462))
REPRESENTATION_CONTEXT('','3D')
);
#5459=(
LENGTH_UNIT()
NAMED_UNIT(*)
SI_UNIT(.CENTI.,.METRE.)
);
#5460=(
LENGTH_UNIT()
NAMED_UNIT(*)
SI_UNIT($,.METRE.)
);
#5461=(
NAMED_UNIT(*)
PLANE_ANGLE_UNIT()
SI_UNIT($,.RADIAN.)
);
#5462=(
NAMED_UNIT(*)
SI_UNIT($,.STERADIAN.)
SOLID_ANGLE_UNIT()
);
#5463=SHAPE_DEFINITION_REPRESENTATION(#5485,#5534);
#5464=SHAPE_DEFINITION_REPRESENTATION(#5486,#5535);
#5465=SHAPE_DEFINITION_REPRESENTATION(#5487,#5536);
#5466=SHAPE_DEFINITION_REPRESENTATION(#5488,#5537);
#5467=SHAPE_DEFINITION_REPRESENTATION(#5489,#5538);
#5468=SHAPE_DEFINITION_REPRESENTATION(#5490,#5539);
#5469=SHAPE_DEFINITION_REPRESENTATION(#5491,#5540);
#5470=SHAPE_DEFINITION_REPRESENTATION(#5492,#5541);
#5471=SHAPE_DEFINITION_REPRESENTATION(#5493,#5542);
#5472=SHAPE_DEFINITION_REPRESENTATION(#5494,#5543);
#5473=SHAPE_DEFINITION_REPRESENTATION(#5495,#5544);
#5474=SHAPE_DEFINITION_REPRESENTATION(#5496,#5545);
#5475=SHAPE_DEFINITION_REPRESENTATION(#5497,#5546);
#5476=SHAPE_DEFINITION_REPRESENTATION(#5499,#5547);
#5477=SHAPE_DEFINITION_REPRESENTATION(#5500,#5548);
#5478=SHAPE_DEFINITION_REPRESENTATION(#5501,#5549);
#5479=SHAPE_DEFINITION_REPRESENTATION(#5502,#5550);
#5480=SHAPE_DEFINITION_REPRESENTATION(#5503,#5551);
#5481=SHAPE_DEFINITION_REPRESENTATION(#5508,#5552);
#5482=SHAPE_DEFINITION_REPRESENTATION(#5518,#5553);
#5483=SHAPE_DEFINITION_REPRESENTATION(#5519,#5554);
#5484=SHAPE_DEFINITION_REPRESENTATION(#5520,#5555);
#5485=PRODUCT_DEFINITION_SHAPE('',$,#5557);
#5486=PRODUCT_DEFINITION_SHAPE('',$,#5558);
#5487=PRODUCT_DEFINITION_SHAPE('',$,#5559);
#5488=PRODUCT_DEFINITION_SHAPE('',$,#5560);
#5489=PRODUCT_DEFINITION_SHAPE('',$,#5561);
#5490=PRODUCT_DEFINITION_SHAPE('',$,#5562);
#5491=PRODUCT_DEFINITION_SHAPE('',$,#5563);
#5492=PRODUCT_DEFINITION_SHAPE('',$,#5564);
#5493=PRODUCT_DEFINITION_SHAPE('',$,#5565);
#5494=PRODUCT_DEFINITION_SHAPE('',$,#5566);
#5495=PRODUCT_DEFINITION_SHAPE('',$,#5567);
#5496=PRODUCT_DEFINITION_SHAPE('',$,#5568);
#5497=PRODUCT_DEFINITION_SHAPE('',$,#5569);
#5498=PRODUCT_DEFINITION_SHAPE($,$,#100);
#5499=PRODUCT_DEFINITION_SHAPE('',$,#5570);
#5500=PRODUCT_DEFINITION_SHAPE('',$,#5571);
#5501=PRODUCT_DEFINITION_SHAPE('',$,#5572);
#5502=PRODUCT_DEFINITION_SHAPE('',$,#5573);
#5503=PRODUCT_DEFINITION_SHAPE('',$,#5574);
#5504=PRODUCT_DEFINITION_SHAPE($,$,#101);
#5505=PRODUCT_DEFINITION_SHAPE($,$,#102);
#5506=PRODUCT_DEFINITION_SHAPE($,$,#103);
#5507=PRODUCT_DEFINITION_SHAPE($,$,#104);
#5508=PRODUCT_DEFINITION_SHAPE('',$,#5575);
#5509=PRODUCT_DEFINITION_SHAPE($,$,#105);
#5510=PRODUCT_DEFINITION_SHAPE($,$,#106);
#5511=PRODUCT_DEFINITION_SHAPE($,$,#107);
#5512=PRODUCT_DEFINITION_SHAPE($,$,#108);
#5513=PRODUCT_DEFINITION_SHAPE($,$,#109);
#5514=PRODUCT_DEFINITION_SHAPE($,$,#110);
#5515=PRODUCT_DEFINITION_SHAPE($,$,#111);
#5516=PRODUCT_DEFINITION_SHAPE($,$,#112);
#5517=PRODUCT_DEFINITION_SHAPE($,$,#113);
#5518=PRODUCT_DEFINITION_SHAPE('',$,#5576);
#5519=PRODUCT_DEFINITION_SHAPE('',$,#5577);
#5520=PRODUCT_DEFINITION_SHAPE('',$,#5578);
#5521=PRODUCT_DEFINITION_SHAPE($,$,#114);
#5522=PRODUCT_DEFINITION_SHAPE($,$,#115);
#5523=PRODUCT_DEFINITION_SHAPE($,$,#116);
#5524=PRODUCT_DEFINITION_SHAPE($,$,#117);
#5525=PRODUCT_DEFINITION_SHAPE($,$,#118);
#5526=PRODUCT_DEFINITION_SHAPE($,$,#119);
#5527=PRODUCT_DEFINITION_SHAPE($,$,#120);
#5528=PRODUCT_DEFINITION_SHAPE($,$,#121);
#5529=PRODUCT_DEFINITION_SHAPE($,$,#122);
#5530=PRODUCT_DEFINITION_SHAPE($,$,#123);
#5531=PRODUCT_DEFINITION_SHAPE($,$,#124);
#5532=PRODUCT_DEFINITION_SHAPE($,$,#125);
#5533=PRODUCT_DEFINITION_SHAPE($,$,#126);
#5534=SHAPE_REPRESENTATION('',(#3176,#3507,#3508,#3509,#3510),#5436);
#5535=SHAPE_REPRESENTATION('',(#3177,#3436,#3437,#3438,#3439),#5437);
#5536=SHAPE_REPRESENTATION('',(#3178),#5438);
#5537=SHAPE_REPRESENTATION('',(#3222),#5439);
#5538=SHAPE_REPRESENTATION('',(#3237),#5440);
#5539=SHAPE_REPRESENTATION('',(#3267,#3451,#3452,#3453,#3454,#3455,#3456,
#3457,#3458,#3459),#5441);
#5540=SHAPE_REPRESENTATION('',(#3268),#5442);
#5541=SHAPE_REPRESENTATION('',(#3296),#5443);
#5542=SHAPE_REPRESENTATION('',(#3305),#5444);
#5543=SHAPE_REPRESENTATION('',(#3314),#5445);
#5544=SHAPE_REPRESENTATION('',(#3324),#5446);
#5545=SHAPE_REPRESENTATION('',(#3348,#3366),#5447);
#5546=SHAPE_REPRESENTATION('',(#3349),#5448);
#5547=SHAPE_REPRESENTATION('',(#3367,#3498,#3499,#3500,#3501,#3502,#3503,
#3504,#3505,#3506),#5449);
#5548=SHAPE_REPRESENTATION('',(#3368),#5450);
#5549=SHAPE_REPRESENTATION('',(#3403),#5451);
#5550=SHAPE_REPRESENTATION('',(#3412),#5452);
#5551=SHAPE_REPRESENTATION('',(#3427),#5453);
#5552=SHAPE_REPRESENTATION('',(#3440),#5454);
#5553=SHAPE_REPRESENTATION('',(#3460),#5455);
#5554=SHAPE_REPRESENTATION('',(#3473),#5456);
#5555=SHAPE_REPRESENTATION('',(#3482),#5457);
#5556=PRODUCT_DEFINITION_CONTEXT('part definition',#5624,'design');
#5557=PRODUCT_DEFINITION('PAT-056','PAT-056',#5579,#5556);
#5558=PRODUCT_DEFINITION('Base and catch plate','Base and catch plate',
#5580,#5556);
#5559=PRODUCT_DEFINITION('Pull-toggle base','Pull-toggle base',#5581,#5556);
#5560=PRODUCT_DEFINITION('Ground pivot screw','Ground pivot screw',#5582,
#5556);
#5561=PRODUCT_DEFINITION('Forked hook catch','Forked hook catch',#5583,
#5556);
#5562=PRODUCT_DEFINITION('Operating handle','Operating handle',#5584,#5556);
#5563=PRODUCT_DEFINITION('Pull-toggle operating lever',
'Pull-toggle operating lever',#5585,#5556);
#5564=PRODUCT_DEFINITION('Pivot spacer 1.8 mm','Pivot spacer 1.8 mm',#5586,
#5556);
#5565=PRODUCT_DEFINITION('Pivot spacer 7 mm','Pivot spacer 7 mm',#5587,
#5556);
#5566=PRODUCT_DEFINITION('Handle','Handle',#5588,#5556);
#5567=PRODUCT_DEFINITION('M5x14 Cap Screw','M5x14 Cap Screw',#5589,#5556);
#5568=PRODUCT_DEFINITION('Offset toggle link','Offset toggle link',#5590,
#5556);
#5569=PRODUCT_DEFINITION('Offset pull link','Offset pull link',#5591,#5556);
#5570=PRODUCT_DEFINITION('Pull crosshead and U-bolt',
'Pull crosshead and U-bolt',#5592,#5556);
#5571=PRODUCT_DEFINITION('Threaded hook crosshead',
'Threaded hook crosshead',#5593,#5556);
#5572=PRODUCT_DEFINITION('Pivot spacer 12.6 mm','Pivot spacer 12.6 mm',
#5594,#5556);
#5573=PRODUCT_DEFINITION('Clevis Pin - 6x30','Clevis Pin - 6x30',#5595,
#5556);
#5574=PRODUCT_DEFINITION('Flat Washer - M6','Flat Washer - M6',#5596,#5556);
#5575=PRODUCT_DEFINITION('Split Pin - 1.6x16','Split Pin - 1.6x16',#5597,
#5556);
#5576=PRODUCT_DEFINITION('Adjustable eight millimetre hook',
'Adjustable eight millimetre hook',#5598,#5556);
#5577=PRODUCT_DEFINITION('Flat Washer - M8','Flat Washer - M8',#5599,#5556);
#5578=PRODUCT_DEFINITION('Hex Nut - M8','Hex Nut - M8',#5600,#5556);
#5579=PRODUCT_DEFINITION_FORMATION('',$,#5626);
#5580=PRODUCT_DEFINITION_FORMATION('',$,#5627);
#5581=PRODUCT_DEFINITION_FORMATION('',$,#5628);
#5582=PRODUCT_DEFINITION_FORMATION('',$,#5629);
#5583=PRODUCT_DEFINITION_FORMATION('',$,#5630);
#5584=PRODUCT_DEFINITION_FORMATION('',$,#5631);
#5585=PRODUCT_DEFINITION_FORMATION('',$,#5632);
#5586=PRODUCT_DEFINITION_FORMATION('',$,#5633);
#5587=PRODUCT_DEFINITION_FORMATION('',$,#5634);
#5588=PRODUCT_DEFINITION_FORMATION('',$,#5635);
#5589=PRODUCT_DEFINITION_FORMATION('',$,#5636);
#5590=PRODUCT_DEFINITION_FORMATION('',$,#5637);
#5591=PRODUCT_DEFINITION_FORMATION('',$,#5638);
#5592=PRODUCT_DEFINITION_FORMATION('',$,#5639);
#5593=PRODUCT_DEFINITION_FORMATION('',$,#5640);
#5594=PRODUCT_DEFINITION_FORMATION('',$,#5641);
#5595=PRODUCT_DEFINITION_FORMATION('',$,#5642);
#5596=PRODUCT_DEFINITION_FORMATION('',$,#5643);
#5597=PRODUCT_DEFINITION_FORMATION('',$,#5644);
#5598=PRODUCT_DEFINITION_FORMATION('',$,#5645);
#5599=PRODUCT_DEFINITION_FORMATION('',$,#5646);
#5600=PRODUCT_DEFINITION_FORMATION('',$,#5647);
#5601=PRODUCT_RELATED_PRODUCT_CATEGORY('PAT-056','PAT-056',(#5626));
#5602=PRODUCT_RELATED_PRODUCT_CATEGORY('Base and catch plate',
'Base and catch plate',(#5627));
#5603=PRODUCT_RELATED_PRODUCT_CATEGORY('Pull-toggle base',
'Pull-toggle base',(#5628));
#5604=PRODUCT_RELATED_PRODUCT_CATEGORY('Ground pivot screw',
'Ground pivot screw',(#5629));
#5605=PRODUCT_RELATED_PRODUCT_CATEGORY('Forked hook catch',
'Forked hook catch',(#5630));
#5606=PRODUCT_RELATED_PRODUCT_CATEGORY('Operating handle',
'Operating handle',(#5631));
#5607=PRODUCT_RELATED_PRODUCT_CATEGORY('Pull-toggle operating lever',
'Pull-toggle operating lever',(#5632));
#5608=PRODUCT_RELATED_PRODUCT_CATEGORY('Pivot spacer 1.8 mm',
'Pivot spacer 1.8 mm',(#5633));
#5609=PRODUCT_RELATED_PRODUCT_CATEGORY('Pivot spacer 7 mm',
'Pivot spacer 7 mm',(#5634));
#5610=PRODUCT_RELATED_PRODUCT_CATEGORY('Handle','Handle',(#5635));
#5611=PRODUCT_RELATED_PRODUCT_CATEGORY('M5x14 Cap Screw',
'M5x14 Cap Screw',(#5636));
#5612=PRODUCT_RELATED_PRODUCT_CATEGORY('Offset toggle link',
'Offset toggle link',(#5637));
#5613=PRODUCT_RELATED_PRODUCT_CATEGORY('Offset pull link',
'Offset pull link',(#5638));
#5614=PRODUCT_RELATED_PRODUCT_CATEGORY('Pull crosshead and U-bolt',
'Pull crosshead and U-bolt',(#5639));
#5615=PRODUCT_RELATED_PRODUCT_CATEGORY('Threaded hook crosshead',
'Threaded hook crosshead',(#5640));
#5616=PRODUCT_RELATED_PRODUCT_CATEGORY('Pivot spacer 12.6 mm',
'Pivot spacer 12.6 mm',(#5641));
#5617=PRODUCT_RELATED_PRODUCT_CATEGORY('Clevis Pin - 6x30',
'Clevis Pin - 6x30',(#5642));
#5618=PRODUCT_RELATED_PRODUCT_CATEGORY('Flat Washer - M6',
'Flat Washer - M6',(#5643));
#5619=PRODUCT_RELATED_PRODUCT_CATEGORY('Split Pin - 1.6x16',
'Split Pin - 1.6x16',(#5644));
#5620=PRODUCT_RELATED_PRODUCT_CATEGORY(
'Adjustable eight millimetre hook','Adjustable eight millimetre hook',(#5645));
#5621=PRODUCT_RELATED_PRODUCT_CATEGORY('Flat Washer - M8',
'Flat Washer - M8',(#5646));
#5622=PRODUCT_RELATED_PRODUCT_CATEGORY('Hex Nut - M8','Hex Nut - M8',(#5647));
#5623=APPLICATION_PROTOCOL_DEFINITION('international standard',
'automotive_design',2009,#5624);
#5624=APPLICATION_CONTEXT(
'Core Data for Automotive Mechanical Design Process');
#5625=PRODUCT_CONTEXT('part definition',#5624,'mechanical');
#5626=PRODUCT('PAT-056','PAT-056','PAT-056',(#5625));
#5627=PRODUCT('Base and catch plate','Base and catch plate',
'Base and catch plate',(#5625));
#5628=PRODUCT('Pull-toggle base','Pull-toggle base','Pull-toggle base',
(#5625));
#5629=PRODUCT('Ground pivot screw','Ground pivot screw',
'Ground pivot screw',(#5625));
#5630=PRODUCT('Forked hook catch','Forked hook catch',
'Forked hook catch',(#5625));
#5631=PRODUCT('Operating handle','Operating handle','Operating handle',
(#5625));
#5632=PRODUCT('Pull-toggle operating lever',
'Pull-toggle operating lever','Pull-toggle operating lever',(#5625));
#5633=PRODUCT('Pivot spacer 1.8 mm','Pivot spacer 1.8 mm',
'Pivot spacer 1.8 mm',(#5625));
#5634=PRODUCT('Pivot spacer 7 mm','Pivot spacer 7 mm',
'Pivot spacer 7 mm',(#5625));
#5635=PRODUCT('Handle','Handle','Handle',(#5625));
#5636=PRODUCT('M5x14 Cap Screw','M5x14 Cap Screw','M5x14 Cap Screw',(#5625));
#5637=PRODUCT('Offset toggle link','Offset toggle link',
'Offset toggle link',(#5625));
#5638=PRODUCT('Offset pull link','Offset pull link','Offset pull link',
(#5625));
#5639=PRODUCT('Pull crosshead and U-bolt','Pull crosshead and U-bolt',
'Pull crosshead and U-bolt',(#5625));
#5640=PRODUCT('Threaded hook crosshead','Threaded hook crosshead',
'Threaded hook crosshead',(#5625));
#5641=PRODUCT('Pivot spacer 12.6 mm','Pivot spacer 12.6 mm',
'Pivot spacer 12.6 mm',(#5625));
#5642=PRODUCT('Clevis Pin - 6x30','Clevis Pin - 6x30',
'Clevis Pin - 6x30',(#5625));
#5643=PRODUCT('Flat Washer - M6','Flat Washer - M6','Flat Washer - M6',
(#5625));
#5644=PRODUCT('Split Pin - 1.6x16','Split Pin - 1.6x16',
'Split Pin - 1.6x16',(#5625));
#5645=PRODUCT('Adjustable eight millimetre hook',
'Adjustable eight millimetre hook','Adjustable eight millimetre hook',(#5625));
#5646=PRODUCT('Flat Washer - M8','Flat Washer - M8','Flat Washer - M8',
(#5625));
#5647=PRODUCT('Hex Nut - M8','Hex Nut - M8','Hex Nut - M8',(#5625));
#5648=PRESENTATION_STYLE_ASSIGNMENT((#5654));
#5649=PRESENTATION_STYLE_ASSIGNMENT((#5655));
#5650=PRESENTATION_STYLE_ASSIGNMENT((#5656));
#5651=PRESENTATION_STYLE_ASSIGNMENT((#5657));
#5652=PRESENTATION_STYLE_ASSIGNMENT((#5658));
#5653=PRESENTATION_STYLE_ASSIGNMENT((#5659));
#5654=SURFACE_STYLE_USAGE(.BOTH.,#5660);
#5655=SURFACE_STYLE_USAGE(.BOTH.,#5661);
#5656=SURFACE_STYLE_USAGE(.BOTH.,#5662);
#5657=SURFACE_STYLE_USAGE(.BOTH.,#5663);
#5658=SURFACE_STYLE_USAGE(.BOTH.,#5664);
#5659=SURFACE_STYLE_USAGE(.BOTH.,#5665);
#5660=SURFACE_SIDE_STYLE('',(#5666));
#5661=SURFACE_SIDE_STYLE('',(#5667));
#5662=SURFACE_SIDE_STYLE('',(#5668));
#5663=SURFACE_SIDE_STYLE('',(#5669));
#5664=SURFACE_SIDE_STYLE('',(#5670));
#5665=SURFACE_SIDE_STYLE('',(#5671));
#5666=SURFACE_STYLE_FILL_AREA(#5672);
#5667=SURFACE_STYLE_FILL_AREA(#5673);
#5668=SURFACE_STYLE_FILL_AREA(#5674);
#5669=SURFACE_STYLE_FILL_AREA(#5675);
#5670=SURFACE_STYLE_FILL_AREA(#5676);
#5671=SURFACE_STYLE_FILL_AREA(#5677);
#5672=FILL_AREA_STYLE('Steel - Satin',(#5678));
#5673=FILL_AREA_STYLE('CAD Library Painted - Deep blue',(#5679));
#5674=FILL_AREA_STYLE('CAD Library Painted - Graphite',(#5680));
#5675=FILL_AREA_STYLE('CAD Library Painted - Engineering blue',(#5681));
#5676=FILL_AREA_STYLE('CAD Library Painted - Light blue',(#5682));
#5677=FILL_AREA_STYLE('CAD Library Painted - Steel gray',(#5683));
#5678=FILL_AREA_STYLE_COLOUR('Steel - Satin',#5684);
#5679=FILL_AREA_STYLE_COLOUR('CAD Library Painted - Deep blue',#5685);
#5680=FILL_AREA_STYLE_COLOUR('CAD Library Painted - Graphite',#5686);
#5681=FILL_AREA_STYLE_COLOUR('CAD Library Painted - Engineering blue',#5687);
#5682=FILL_AREA_STYLE_COLOUR('CAD Library Painted - Light blue',#5688);
#5683=FILL_AREA_STYLE_COLOUR('CAD Library Painted - Steel gray',#5689);
#5684=COLOUR_RGB('Steel - Satin',0.627450980392157,0.627450980392157,0.627450980392157);
#5685=COLOUR_RGB('CAD Library Painted - Deep blue',0.0784313725490196,0.203921568627451,
0.349019607843137);
#5686=COLOUR_RGB('CAD Library Painted - Graphite',0.0980392156862745,0.109803921568627,
0.125490196078431);
#5687=COLOUR_RGB('CAD Library Painted - Engineering blue',0.12156862745098,
0.356862745098039,0.6);
#5688=COLOUR_RGB('CAD Library Painted - Light blue',0.286274509803922,0.552941176470588,
0.780392156862745);
#5689=COLOUR_RGB('CAD Library Painted - Steel gray',0.592156862745098,0.631372549019608,
0.67843137254902);
#5690=COLOUR_RGB('Dark Blue',0.08,0.2,0.34);
#5691=FILL_AREA_STYLE_COLOUR('',#5690);
#5692=FILL_AREA_STYLE('',(#5691));
#5693=SURFACE_STYLE_FILL_AREA(#5692);
#5694=SURFACE_SIDE_STYLE('',(#5693));
#5695=SURFACE_STYLE_USAGE(.BOTH.,#5694);
#5696=PRESENTATION_STYLE_ASSIGNMENT((#5695));
#5697=COLOUR_RGB('Light Blue',0.38,0.62,0.78);
#5698=FILL_AREA_STYLE_COLOUR('',#5697);
#5699=FILL_AREA_STYLE('',(#5698));
#5700=SURFACE_STYLE_FILL_AREA(#5699);
#5701=SURFACE_SIDE_STYLE('',(#5700));
#5702=SURFACE_STYLE_USAGE(.BOTH.,#5701);
#5703=PRESENTATION_STYLE_ASSIGNMENT((#5702));
#5704=COLOUR_RGB('Sky Blue',0.24,0.69,0.87);
#5705=FILL_AREA_STYLE_COLOUR('',#5704);
#5706=FILL_AREA_STYLE('',(#5705));
#5707=SURFACE_STYLE_FILL_AREA(#5706);
#5708=SURFACE_SIDE_STYLE('',(#5707));
#5709=SURFACE_STYLE_USAGE(.BOTH.,#5708);
#5710=PRESENTATION_STYLE_ASSIGNMENT((#5709));
#5711=COLOUR_RGB('Grey',0.48,0.52,0.57);
#5712=FILL_AREA_STYLE_COLOUR('',#5711);
#5713=FILL_AREA_STYLE('',(#5712));
#5714=SURFACE_STYLE_FILL_AREA(#5713);
#5715=SURFACE_SIDE_STYLE('',(#5714));
#5716=SURFACE_STYLE_USAGE(.BOTH.,#5715);
#5717=PRESENTATION_STYLE_ASSIGNMENT((#5716));
#5718=COLOUR_RGB('Black',0.12,0.14,0.17);
#5719=FILL_AREA_STYLE_COLOUR('',#5718);
#5720=FILL_AREA_STYLE('',(#5719));
#5721=SURFACE_STYLE_FILL_AREA(#5720);
#5722=SURFACE_SIDE_STYLE('',(#5721));
#5723=SURFACE_STYLE_USAGE(.BOTH.,#5722);
#5724=PRESENTATION_STYLE_ASSIGNMENT((#5723));
#5725=COLOUR_RGB('Off White',0.89,0.88,0.83);
#5726=FILL_AREA_STYLE_COLOUR('',#5725);
#5727=FILL_AREA_STYLE('',(#5726));
#5728=SURFACE_STYLE_FILL_AREA(#5727);
#5729=SURFACE_SIDE_STYLE('',(#5728));
#5730=SURFACE_STYLE_USAGE(.BOTH.,#5729);
#5731=PRESENTATION_STYLE_ASSIGNMENT((#5730));
ENDSEC;
END-ISO-10303-21;
